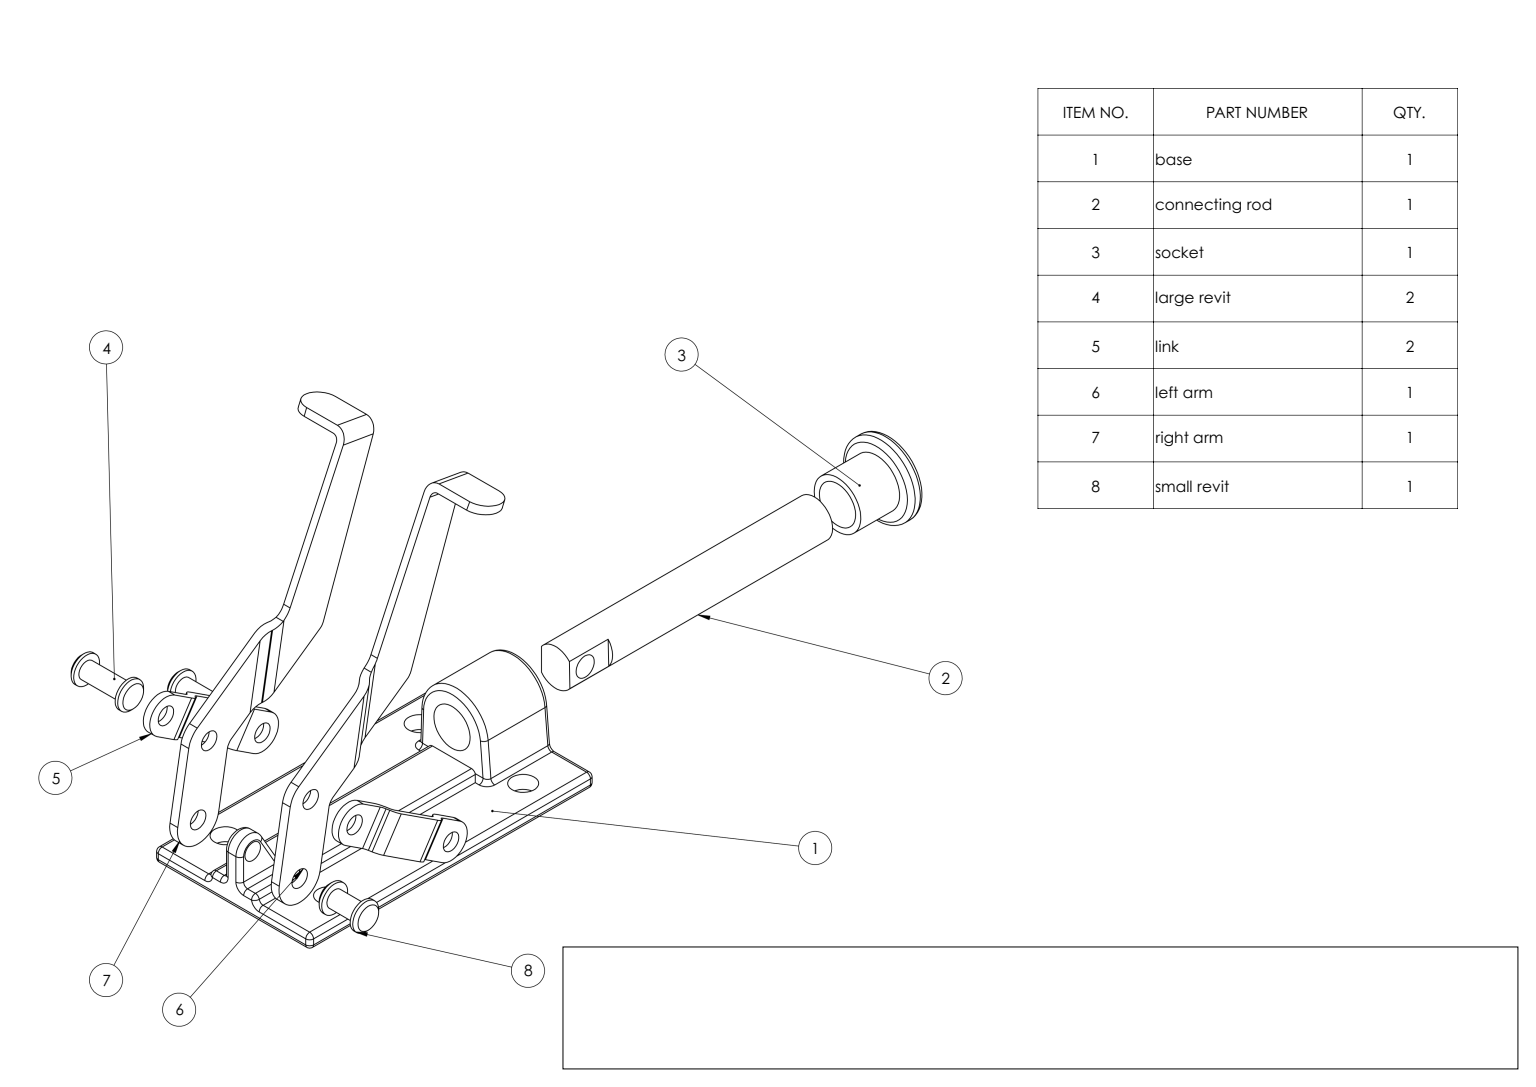
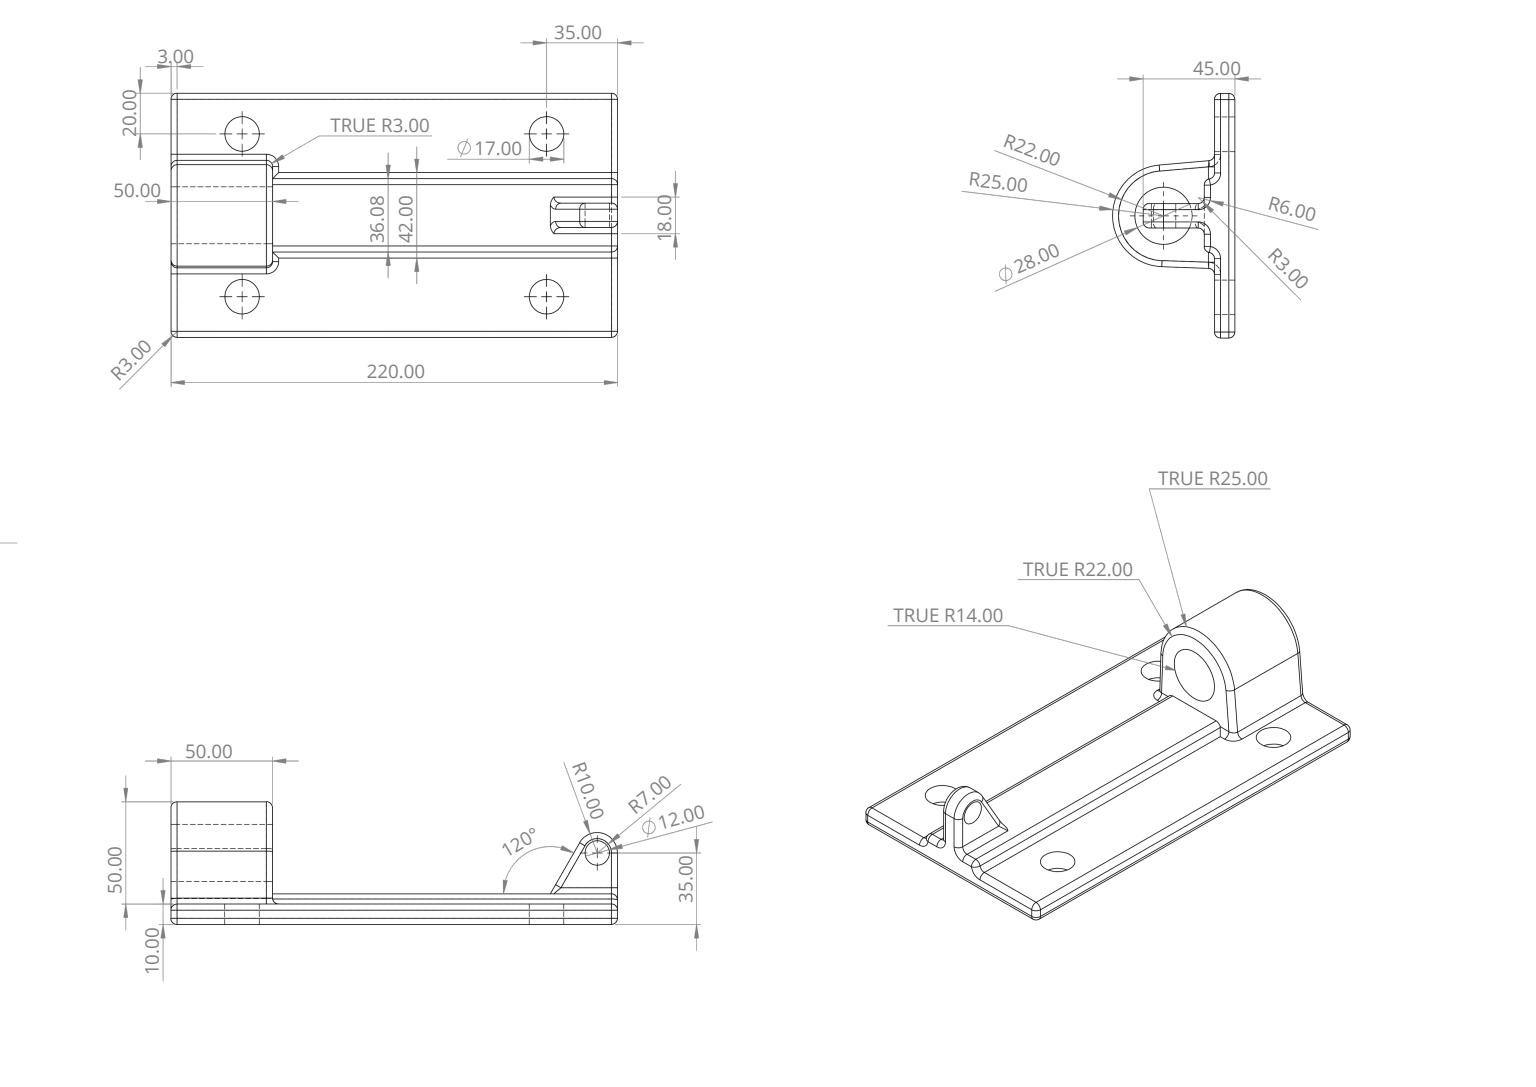
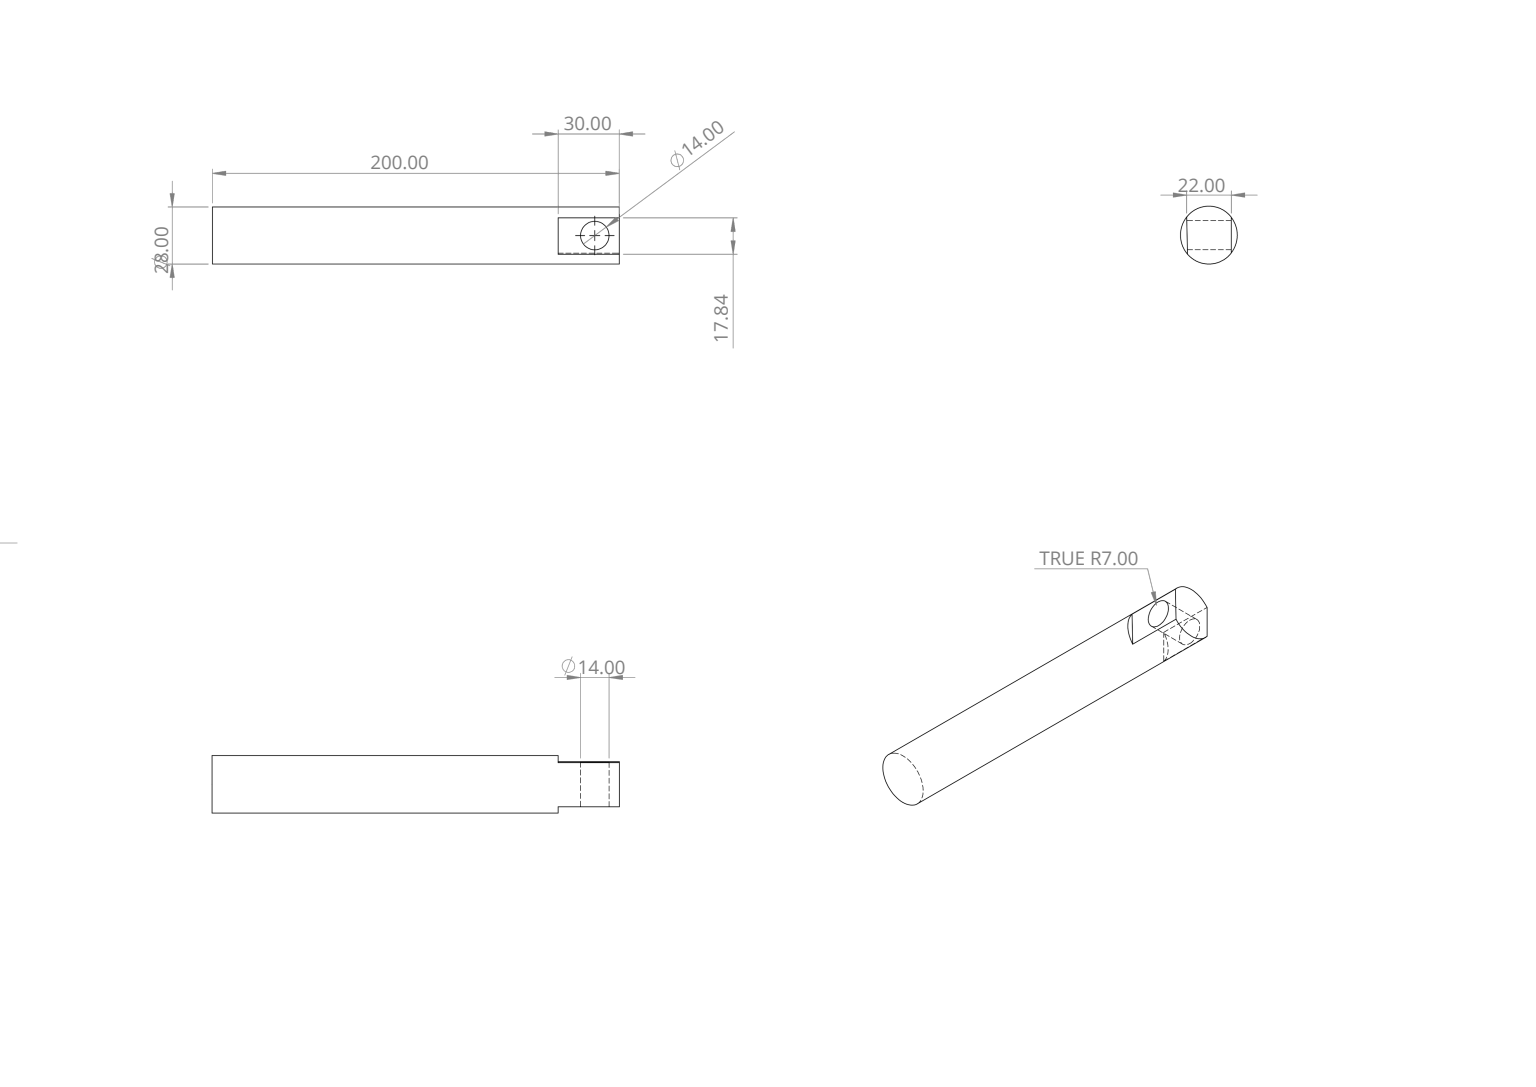
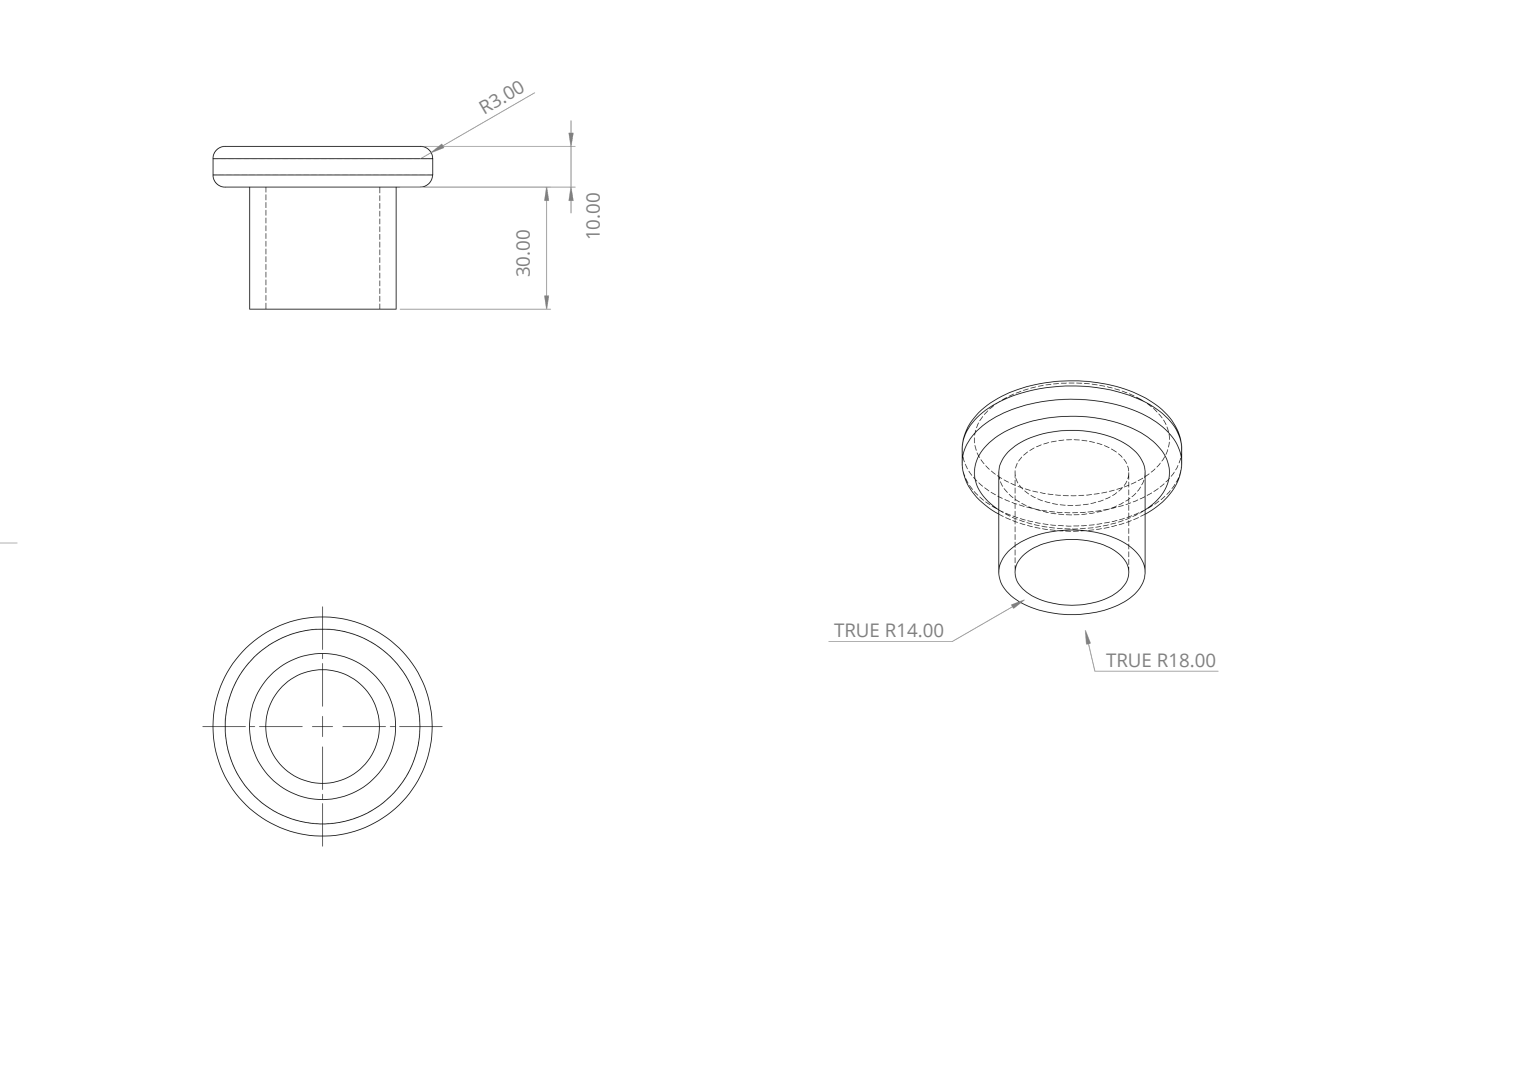
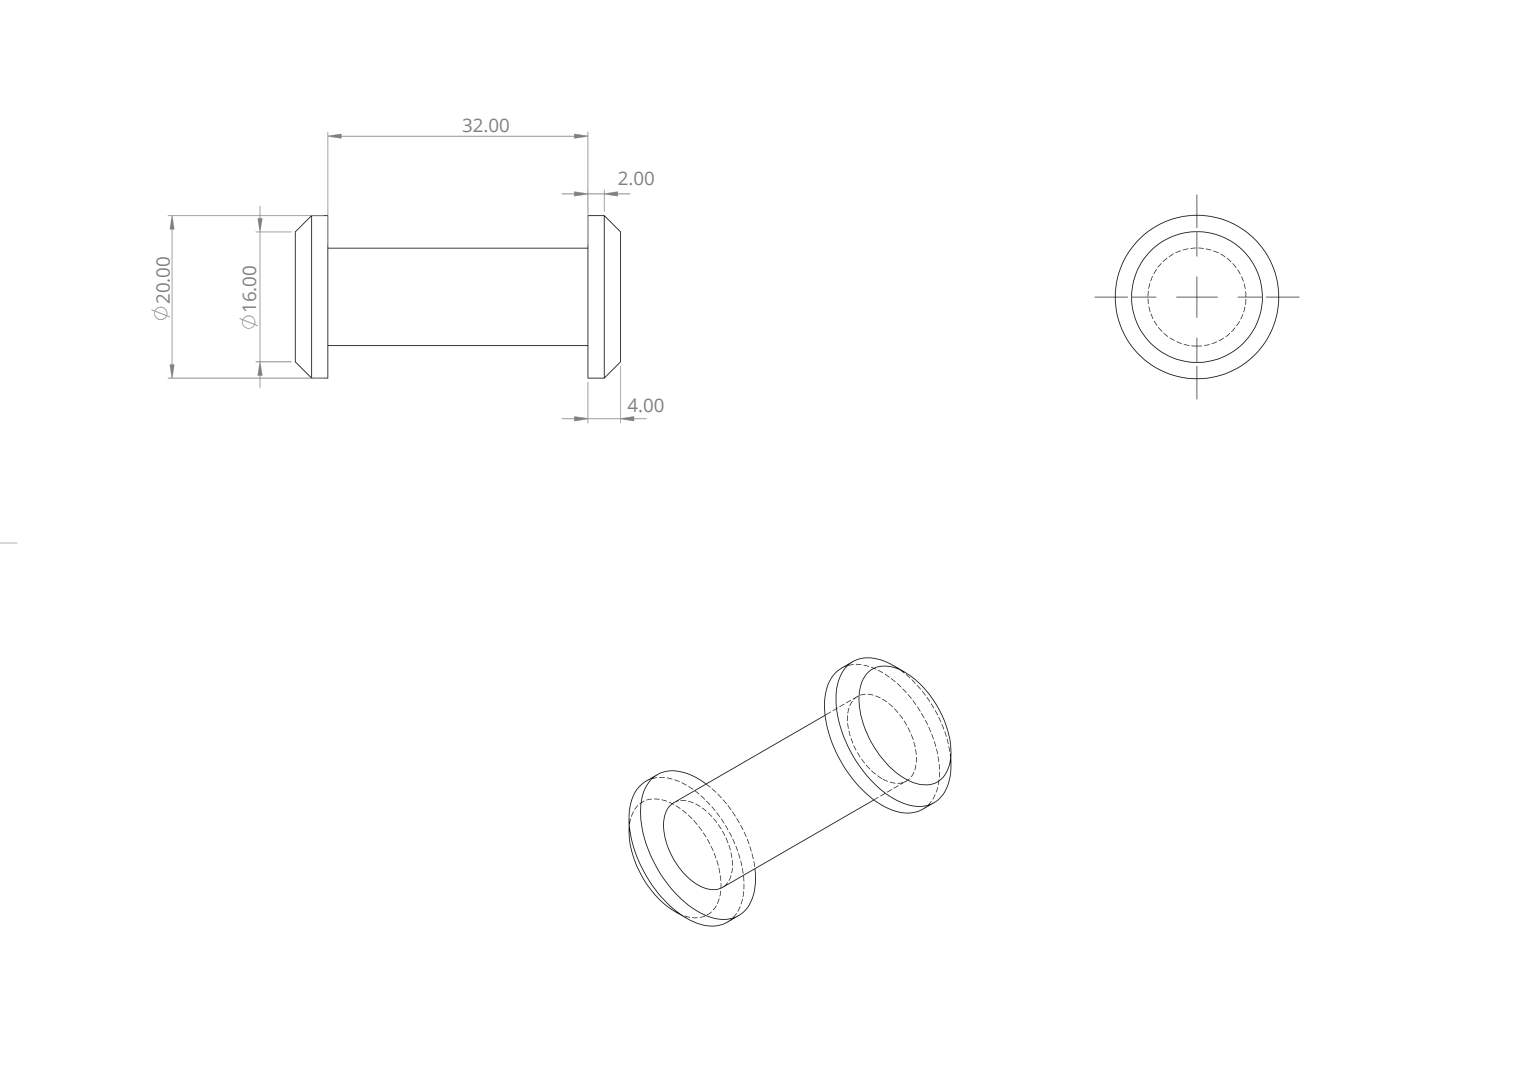
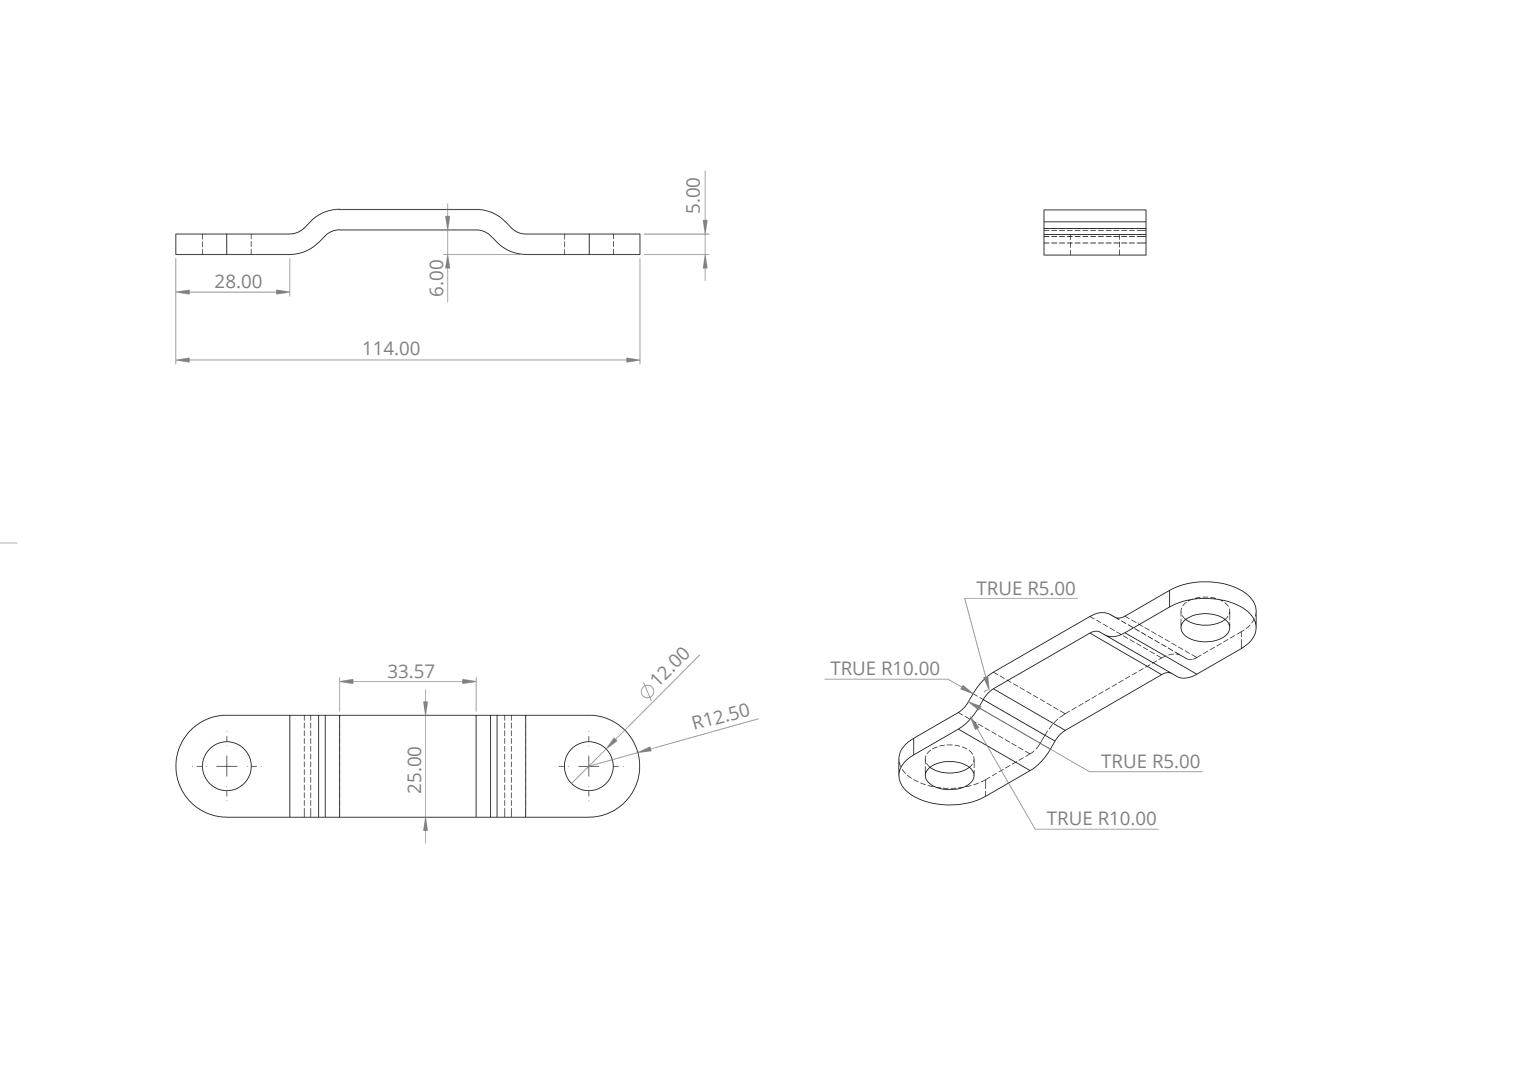
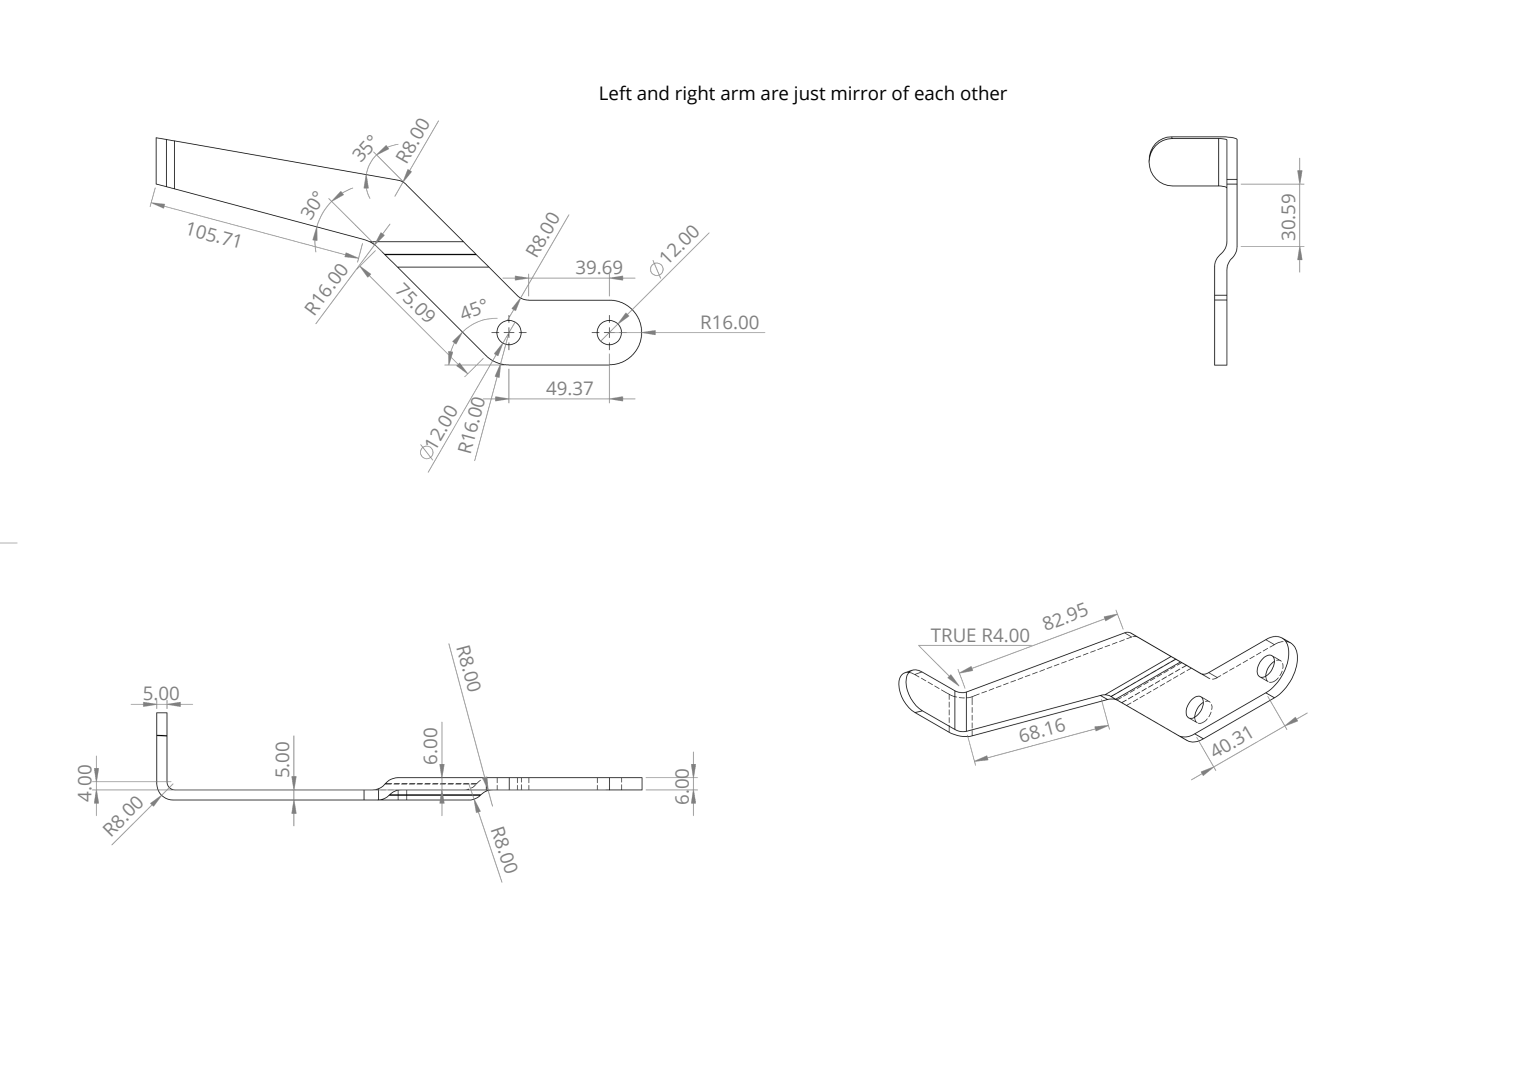
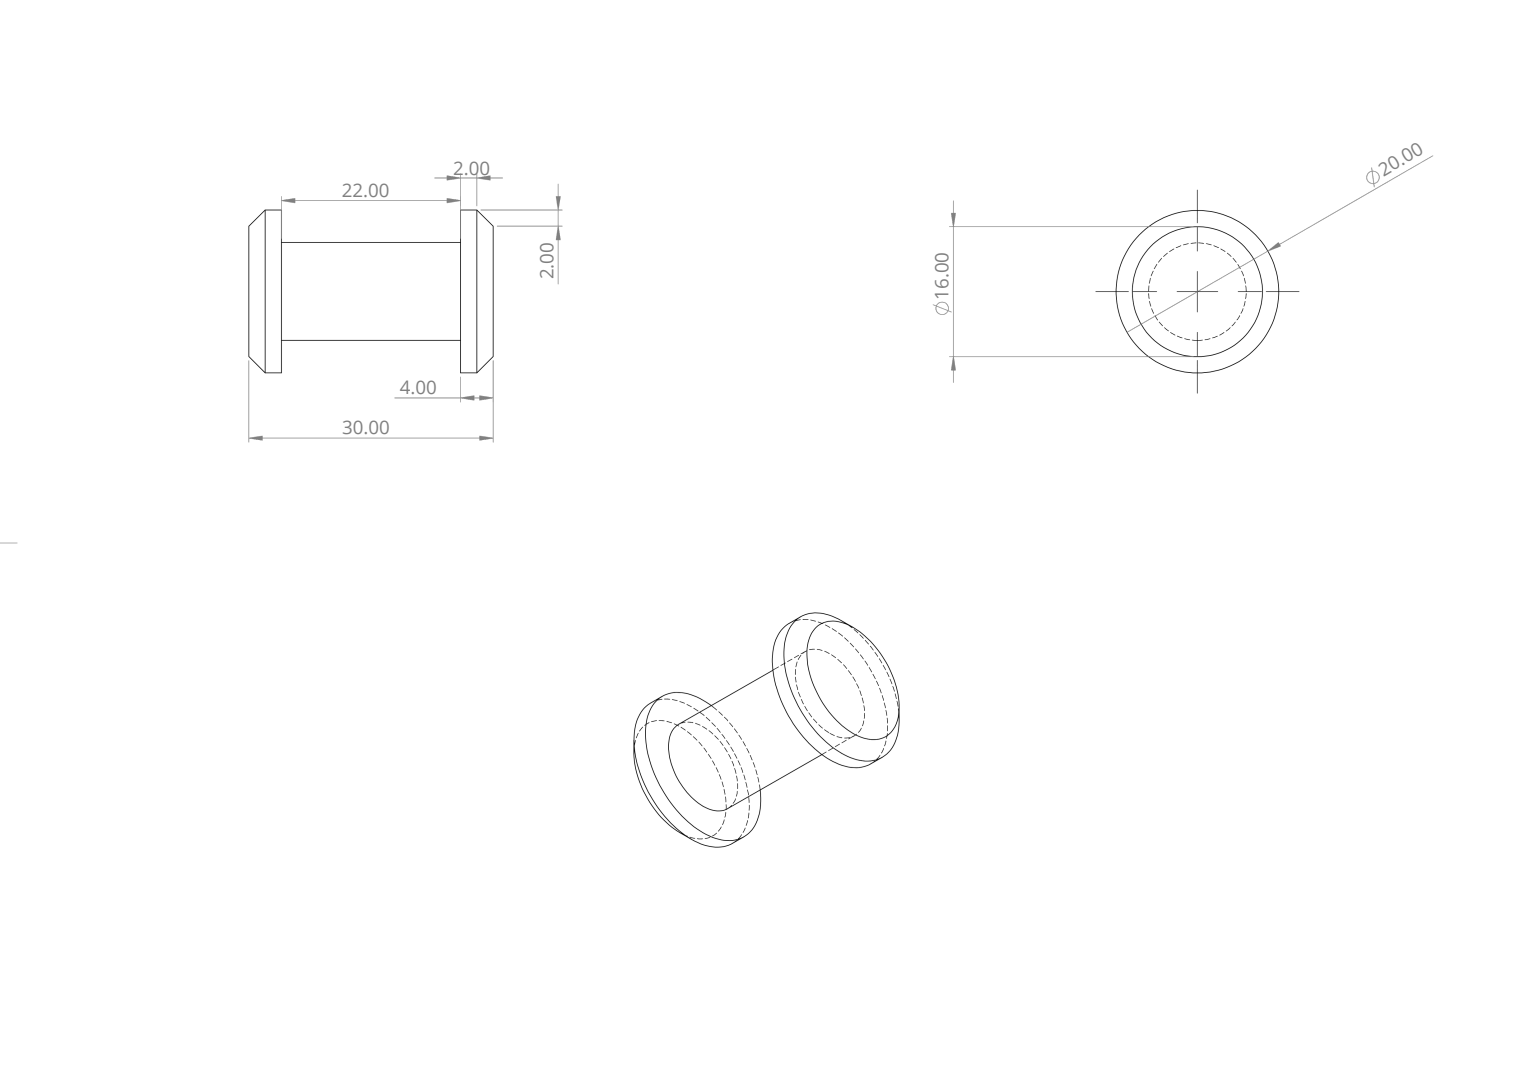
ISO-10303-21;
HEADER;
FILE_DESCRIPTION (('STEP AP214'),
    '1' );
FILE_NAME ('MAT-051',
    '2026-10-28T16:30:29',
    ( '' ),
    ( '' ),
    'SwSTEP 2.0',
    'SolidWorks 2025',
    '' );
FILE_SCHEMA (( 'AUTOMOTIVE_DESIGN' ));
ENDSEC;

DATA;
#1 = ORIENTED_EDGE ( 'NONE', *, *, #6027, .T. ) ;
#2 = AXIS2_PLACEMENT_3D ( 'NONE', #7401, #6721, #5569 ) ;
#3 = VERTEX_POINT ( 'NONE', #4491 ) ;
#4 = VECTOR ( 'NONE', #6644, 1000.000000000000000 ) ;
#5 = ADVANCED_FACE ( 'NONE', ( #5063 ), #903, .F. ) ;
#6 = CARTESIAN_POINT ( 'NONE',  ( -16.49999999999998934, 16.00000000000003908, 44.76505905230379767 ) ) ;
#7 = CARTESIAN_POINT ( 'NONE',  ( 27.24881022415626575, -213.6786602093778242, 88.60457046541063164 ) ) ;
#8 = ORIENTED_EDGE ( 'NONE', *, *, #2095, .F. ) ;
#9 = EDGE_CURVE ( 'NONE', #2534, #191, #5287, .T. ) ;
#10 = PRODUCT_CONTEXT ( 'NONE', #4822, 'mechanical' ) ;
#11 = AXIS2_PLACEMENT_3D ( 'NONE', #6403, #3479, #547 ) ;
#12 = DIRECTION ( 'NONE',  ( 1.000000000000000000, 0.000000000000000000, 0.000000000000000000 ) ) ;
#13 = EDGE_LOOP ( 'NONE', ( #3955, #3926, #2198, #6587 ) ) ;
#14 = AXIS2_PLACEMENT_3D ( 'NONE', #4631, #3929, #1078 ) ;
#15 = DIRECTION ( 'NONE',  ( 0.000000000000000000, 1.301042606982607490E-15, -1.000000000000000000 ) ) ;
#16 = DIRECTION ( 'NONE',  ( 1.000000000000000000, 0.000000000000000000, 0.000000000000000000 ) ) ;
#17 = CARTESIAN_POINT ( 'NONE',  ( 20.98347821072601960, -218.0630240738405519, 87.23510494545232064 ) ) ;
#18 = CARTESIAN_POINT ( 'NONE',  ( 20.97288657943079571, -223.0630240738404382, 88.26575131447681599 ) ) ;
#19 = CARTESIAN_POINT ( 'NONE',  ( -17.32280336819468047, -61.82280336819459166, 34.82280336819469824 ) ) ;
#20 = EDGE_CURVE ( 'NONE', #1964, #6977, #5721, .T. ) ;
#21 = PRODUCT_DEFINITION_CONTEXT ( 'detailed design', #2454, 'design' ) ;
#22 = EDGE_LOOP ( 'NONE', ( #2076, #4866, #387, #2753, #42, #1784, #2773 ) ) ;
#23 = AXIS2_PLACEMENT_3D ( 'NONE', #5950, #680, #1328 ) ;
#24 = ORIENTED_EDGE ( 'NONE', *, *, #3857, .T. ) ;
#25 = SURFACE_STYLE_FILL_AREA ( #599 ) ;
#26 = CARTESIAN_POINT ( 'NONE',  ( 3.000000000000002665, 0.000000000000000000, 35.00000000000000000 ) ) ;
#27 = LINE ( 'NONE', #5419, #4744 ) ;
#28 = CARTESIAN_POINT ( 'NONE',  ( 188.6380400399839061, 9.000000000000001776, 15.00000000000000888 ) ) ;
#29 = CARTESIAN_POINT ( 'NONE',  ( 30.00000000000000000, 0.000000000000000000, 0.000000000000000000 ) ) ;
#30 = AXIS2_PLACEMENT_3D ( 'NONE', #3464, #4542, #1564 ) ;
#31 = ORIENTED_EDGE ( 'NONE', *, *, #3655, .T. ) ;
#32 = ORIENTED_EDGE ( 'NONE', *, *, #3252, .F. ) ;
#33 = FACE_OUTER_BOUND ( 'NONE', #3649, .T. ) ;
#34 = DIRECTION ( 'NONE',  ( 1.000000000000000000, 2.465190328815661892E-32, -9.244463733058732095E-33 ) ) ;
#35 = ORIENTED_EDGE ( 'NONE', *, *, #1878, .T. ) ;
#36 = LINE ( 'NONE', #2385, #2482 ) ;
#37 = EDGE_CURVE ( 'NONE', #4344, #2575, #5917, .T. ) ;
#38 = SURFACE_STYLE_FILL_AREA ( #2961 ) ;
#39 = CARTESIAN_POINT ( 'NONE',  ( 200.0000000000000000, 11.00000000000000711, 8.660254037844383745 ) ) ;
#40 = EDGE_CURVE ( 'NONE', #3862, #1645, #5779, .T. ) ;
#41 = EDGE_LOOP ( 'NONE', ( #5508, #4352, #6797, #4752 ) ) ;
#42 = ORIENTED_EDGE ( 'NONE', *, *, #4968, .F. ) ;
#43 = AXIS2_PLACEMENT_3D ( 'NONE', #7599, #4696, #644 ) ;
#44 = PRODUCT_DEFINITION_SHAPE ( 'NONE', 'NONE',  #7602 ) ;
#45 = AXIS2_PLACEMENT_3D ( 'NONE', #5549, #210, #1347 ) ;
#46 = CARTESIAN_POINT ( 'NONE',  ( 209.9999999999999716, -3.000000000000000888, 35.00000000000000000 ) ) ;
#47 = CARTESIAN_POINT ( 'NONE',  ( 4.000000000000003553, 0.000000000000000000, 1.387778780781445676E-14 ) ) ;
#48 = ORIENTED_EDGE ( 'NONE', *, *, #3226, .T. ) ;
#49 = SHAPE_DEFINITION_REPRESENTATION ( #3722, #915 ) ;
#50 = DIRECTION ( 'NONE',  ( -1.000000000000000000, -0.000000000000000000, -0.000000000000000000 ) ) ;
#51 = DIRECTION ( 'NONE',  ( -1.084202172485505174E-16, 0.000000000000000000, 1.000000000000000000 ) ) ;
#52 = AXIS2_PLACEMENT_3D ( 'NONE', #1456, #3815, #1490 ) ;
#53 = AXIS2_PLACEMENT_3D ( 'NONE', #1297, #6992, #2338 ) ;
#54 = EDGE_CURVE ( 'NONE', #3265, #5898, #5654, .T. ) ;
#55 = ADVANCED_FACE ( 'NONE', ( #5029 ), #3220, .F. ) ;
#56 = ORIENTED_EDGE ( 'NONE', *, *, #1998, .T. ) ;
#57 = DIRECTION ( 'NONE',  ( 1.000000000000000000, 0.000000000000000000, 5.605193857299269528E-45 ) ) ;
#58 = CONICAL_SURFACE ( 'NONE', #5587, 8.000000000000003553, 0.7853981633974447263 ) ;
#59 = CARTESIAN_POINT ( 'NONE',  ( 30.00000000000000000, 0.000000000000000000, 0.000000000000000000 ) ) ;
#60 = CIRCLE ( 'NONE', #2634, 6.000000000000000888 ) ;
#61 = EDGE_LOOP ( 'NONE', ( #832, #7441, #3199, #4016 ) ) ;
#62 = DIRECTION ( 'NONE',  ( 0.000000000000000000, 0.000000000000000000, 1.000000000000000000 ) ) ;
#63 = CARTESIAN_POINT ( 'NONE',  ( 21.48754873573582813, -218.0630240738405803, 84.27726093503913773 ) ) ;
#64 = CARTESIAN_POINT ( 'NONE',  ( 3.000000000000002665, 30.03170604878415162, 13.00000000000001066 ) ) ;
#65 = FACE_OUTER_BOUND ( 'NONE', #2315, .T. ) ;
#66 = VECTOR ( 'NONE', #761, 1000.000000000000000 ) ;
#67 = TOROIDAL_SURFACE ( 'NONE', #1523, 24.00000000000000000, 3.000000000000000000 ) ;
#68 = VECTOR ( 'NONE', #7179, 1000.000000000000000 ) ;
#69 = ORIENTED_EDGE ( 'NONE', *, *, #4461, .T. ) ;
#70 = DIRECTION ( 'NONE',  ( -1.368455531567204171E-48, -0.1736481776669304422, -0.9848077530122080203 ) ) ;
#71 = CARTESIAN_POINT ( 'NONE',  ( 4.000000000000003553, 0.000000000000000000, 1.387778780781445676E-14 ) ) ;
#72 = DIRECTION ( 'NONE',  ( 0.000000000000000000, -0.03489949670250429292, -0.9993908270190956511 ) ) ;
#73 = PLANE ( 'NONE',  #5716 ) ;
#74 = DIRECTION ( 'NONE',  ( 0.000000000000000000, 0.000000000000000000, -1.000000000000000000 ) ) ;
#75 = AXIS2_PLACEMENT_3D ( 'NONE', #6050, #2005, #4940 ) ;
#76 = PRODUCT_DEFINITION_FORMATION_WITH_SPECIFIED_SOURCE ( 'ANY', '', #2239, .NOT_KNOWN. ) ;
#77 = CARTESIAN_POINT ( 'NONE',  ( 187.7594781219628999, -3.757281668791117468, 16.47828612039246465 ) ) ;
#78 = EDGE_LOOP ( 'NONE', ( #6432, #8, #7430, #5841, #2401, #1388, #6356, #5368 ) ) ;
#79 = VERTEX_POINT ( 'NONE', #3915 ) ;
#80 = EDGE_CURVE ( 'NONE', #4729, #1895, #4308, .T. ) ;
#81 = DIRECTION ( 'NONE',  ( -1.000000000000000000, 0.000000000000000000, -7.663350976776343357E-46 ) ) ;
#82 = CARTESIAN_POINT ( 'NONE',  ( 220.0000000000000000, -56.99999999999999289, 7.000000000000000888 ) ) ;
#83 = ORIENTED_EDGE ( 'NONE', *, *, #275, .T. ) ;
#84 = CARTESIAN_POINT ( 'NONE',  ( -53.48785751550376233, -228.1620966263577657, 74.64757051591519144 ) ) ;
#85 = AXIS2_PLACEMENT_3D ( 'NONE', #4576, #2304, #5803 ) ;
#86 = CARTESIAN_POINT ( 'NONE',  ( -30.49999999999998579, -218.0630240738404950, 95.20959099461346398 ) ) ;
#87 = DIRECTION ( 'NONE',  ( 1.000000000000000000, 0.000000000000000000, 0.000000000000000000 ) ) ;
#88 = ORIENTED_EDGE ( 'NONE', *, *, #483, .F. ) ;
#89 = ORIENTED_EDGE ( 'NONE', *, *, #875, .F. ) ;
#90 = AXIS2_PLACEMENT_3D ( 'NONE', #1507, #1400, #825 ) ;
#91 = EDGE_CURVE ( 'NONE', #2680, #1796, #4925, .T. ) ;
#92 = FACE_BOUND ( 'NONE', #5400, .T. ) ;
#93 = CARTESIAN_POINT ( 'NONE',  ( 17.75187451922245430, -223.0194114314941203, 73.26959217102432831 ) ) ;
#94 = ORIENTED_EDGE ( 'NONE', *, *, #5676, .T. ) ;
#95 = SHAPE_DEFINITION_REPRESENTATION ( #6712, #867 ) ;
#96 = DIRECTION ( 'NONE',  ( 3.379803290564627601E-16, -1.193489751472043281E-15, 1.000000000000000000 ) ) ;
#97 = SHAPE_REPRESENTATION ( 'socket', ( #1914 ), #434 ) ;
#98 = CARTESIAN_POINT ( 'NONE',  ( 217.0000000000000000, 20.99999999999999645, 13.00000000000000888 ) ) ;
#99 = AXIS2_PLACEMENT_3D ( 'NONE', #6628, #2937, #5286 ) ;
#100 = EDGE_LOOP ( 'NONE', ( #3777, #3352, #1778, #3381, #5909, #4070 ) ) ;
#101 = AXIS2_PLACEMENT_3D ( 'NONE', #3506, #6921, #4007 ) ;
#102 = CARTESIAN_POINT ( 'NONE',  ( -27.00000000000000000, 3.306546357697852550E-15, -3.000000000000002665 ) ) ;
#103 = EDGE_CURVE ( 'NONE', #1980, #3365, #5258, .T. ) ;
#104 = DIRECTION ( 'NONE',  ( -2.465190328815661892E-32, -1.000000000000000000, -1.193489751472043281E-15 ) ) ;
#105 = VERTEX_POINT ( 'NONE', #3335 ) ;
#106 = APPLICATION_CONTEXT ( 'automotive_design' ) ;
#107 = CYLINDRICAL_SURFACE ( 'NONE', #7534, 3.000000000000000000 ) ;
#108 = CARTESIAN_POINT ( 'NONE',  ( 0.000000000000000000, 0.000000000000000000, 0.000000000000000000 ) ) ;
#109 = CARTESIAN_POINT ( 'NONE',  ( 190.0729179104125137, 6.000000000000001776, 16.24264068711929454 ) ) ;
#110 = PLANE ( 'NONE',  #3658 ) ;
#111 = ADVANCED_FACE ( 'NONE', ( #6250 ), #4449, .F. ) ;
#112 = PLANE ( 'NONE',  #4971 ) ;
#113 = DIRECTION ( 'NONE',  ( 5.551115123125785167E-17, -0.7071067811865451302, 0.7071067811865499042 ) ) ;
#114 = CARTESIAN_POINT ( 'NONE',  ( -23.99999999999999289, 2.939152317953645922E-15, -3.000000000000002665 ) ) ;
#115 = CARTESIAN_POINT ( 'NONE',  ( 0.000000000000000000, 0.000000000000000000, 0.000000000000000000 ) ) ;
#116 = DIRECTION ( 'NONE',  ( -5.551115123125785167E-17, 0.7071067811865469066, 0.7071067811865482389 ) ) ;
#117 = ORIENTED_EDGE ( 'NONE', *, *, #841, .F. ) ;
#118 = ORIENTED_EDGE ( 'NONE', *, *, #6512, .T. ) ;
#119 = CARTESIAN_POINT ( 'NONE',  ( 217.0000000000000000, 56.99999999999999289, 2.149255132503604690E-14 ) ) ;
#120 = CARTESIAN_POINT ( 'NONE',  ( 36.00000000000000000, 0.000000000000000000, 1.387778780781445676E-14 ) ) ;
#121 = CARTESIAN_POINT ( 'NONE',  ( -70.24881022415625864, -213.6786602093778527, 88.60457046541068848 ) ) ;
#122 = PLANE ( 'NONE',  #5791 ) ;
#123 = CARTESIAN_POINT ( 'NONE',  ( -57.55570709107922767, -218.0630177787537605, 94.33845620223004858 ) ) ;
#124 = EDGE_CURVE ( 'NONE', #3147, #3862, #1554, .T. ) ;
#125 = ORIENTED_EDGE ( 'NONE', *, *, #2917, .T. ) ;
#126 =( BOUNDED_SURFACE ( )  B_SPLINE_SURFACE ( 3, 2, ( 
 ( #6358, #1115, #535 ),
 ( #7576, #4667, #7000 ),
 ( #5776, #2923, #7425 ),
 ( #2158, #4511, #999 ),
 ( #424, #6970, #2887 ),
 ( #5124, #7466, #686 ),
 ( #2497, #3699, #5310 ),
 ( #4202, #3048, #6003 ),
 ( #6470, #4707, #3588 ),
 ( #1190, #4166, #614 ) ),
 .UNSPECIFIED., .F., .F., .F. ) 
 B_SPLINE_SURFACE_WITH_KNOTS ( ( 4, 2, 2, 2, 4 ),
 ( 3, 3 ),
 ( 1.570796326794896558, 1.963495408493620697, 2.356194490192344837, 2.748893571891068976, 3.141592653589793116 ),
 ( 0.000000000000000000, 1.000000000000000000 ),
 .UNSPECIFIED. ) 
 GEOMETRIC_REPRESENTATION_ITEM ( )  RATIONAL_B_SPLINE_SURFACE ( (
 ( 1.000000000000000000, 0.7071067811865473507, 1.000000000000000000),
 ( 1.000000000000000000, 0.7087223175983969892, 1.000000000000000000),
 ( 1.000000000000000000, 0.7103306498028938432, 1.000000000000000000),
 ( 1.000000000000000000, 0.7132953257861496255, 1.000000000000000000),
 ( 1.000000000000000000, 0.7146502351234478301, 1.000000000000000000),
 ( 1.000000000000000000, 0.7169067290091972744, 1.000000000000000000),
 ( 1.000000000000000000, 0.7178075805514493313, 1.000000000000000000),
 ( 1.000000000000000000, 0.7190243029327590962, 1.000000000000000000),
 ( 1.000000000000000000, 0.7193412045353504425, 1.000000000000000000),
 ( 1.000000000000000000, 0.7193398003386524131, 1.000000000000000000) ) ) 
 REPRESENTATION_ITEM ( '' )  SURFACE ( )  );
#127 = EDGE_LOOP ( 'NONE', ( #2501, #1142, #956, #2609 ) ) ;
#128 = AXIS2_PLACEMENT_3D ( 'NONE', #2301, #7483, #6908 ) ;
#129 = CARTESIAN_POINT ( 'NONE',  ( 43.50000000000001421, 39.99999999999999289, 0.000000000000000000 ) ) ;
#130 = CARTESIAN_POINT ( 'NONE',  ( 27.04900473833201957, -225.0595978535630479, 79.55554317441176693 ) ) ;
#131 = VERTEX_POINT ( 'NONE', #5107 ) ;
#132 = CARTESIAN_POINT ( 'NONE',  ( 47.00000000000000000, 0.000000000000000000, 35.00000000000000000 ) ) ;
#133 = DIRECTION ( 'NONE',  ( 0.000000000000000000, -4.440892098500625373E-15, -1.000000000000000000 ) ) ;
#134 = CLOSED_SHELL ( 'NONE', ( #4385, #2935, #2103, #5773, #2173, #1411, #598, #7589, #2241, #2766, #3161, #4459, #4149, #7376, #3485, #1798, #883, #2489, #2656, #6564, #2581, #4183, #1712, #6059, #2477, #6043 ) ) ;
#135 = VECTOR ( 'NONE', #6601, 1000.000000000000000 ) ;
#136 = ORIENTED_EDGE ( 'NONE', *, *, #2636, .T. ) ;
#137 = DIRECTION ( 'NONE',  ( 0.000000000000000000, -1.000000000000000000, 0.000000000000000000 ) ) ;
#138 = AXIS2_PLACEMENT_3D ( 'NONE', #4135, #4211, #3123 ) ;
#139 = SPHERICAL_SURFACE ( 'NONE', #1773, 3.000000000000000000 ) ;
#140 = CARTESIAN_POINT ( 'NONE',  ( 26.49999999999999645, -39.99999999999999289, 0.000000000000000000 ) ) ;
#141 = FACE_OUTER_BOUND ( 'NONE', #3804, .T. ) ;
#142 = CARTESIAN_POINT ( 'NONE',  ( -16.49999999999996447, -57.68629150101509850, 30.68629150101520509 ) ) ;
#143 = EDGE_CURVE ( 'NONE', #589, #4118, #1720, .T. ) ;
#144 = ORIENTED_EDGE ( 'NONE', *, *, #928, .F. ) ;
#145 = CARTESIAN_POINT ( 'NONE',  ( -64.50000000000000000, -105.5631177942458407, 67.24940929526127320 ) ) ;
#146 = DIRECTION ( 'NONE',  ( 0.000000000000000000, 0.000000000000000000, 1.000000000000000000 ) ) ;
#147 = DIRECTION ( 'NONE',  ( -0.000000000000000000, 1.000000000000000000, 1.836970198721029934E-16 ) ) ;
#148 = LINE ( 'NONE', #4110, #1043 ) ;
#149 = CARTESIAN_POINT ( 'NONE',  ( -56.14779210138475918, -223.0637666356699071, 73.66476142575187680 ) ) ;
#150 = FACE_OUTER_BOUND ( 'NONE', #7477, .T. ) ;
#151 = VECTOR ( 'NONE', #2336, 1000.000000000000000 ) ;
#152 = EDGE_CURVE ( 'NONE', #3617, #6429, #5143, .T. ) ;
#153 = ORIENTED_EDGE ( 'NONE', *, *, #1028, .T. ) ;
#154 = EDGE_LOOP ( 'NONE', ( #6396, #3446, #5097, #6881, #3077, #1951, #4826, #5186 ) ) ;
#155 = DIRECTION ( 'NONE',  ( 1.853902270198407313E-44, 1.000000000000000000, 0.000000000000000000 ) ) ;
#156 = VECTOR ( 'NONE', #2539, 1000.000000000000000 ) ;
#157 = PLANE ( 'NONE',  #5099 ) ;
#158 = CARTESIAN_POINT ( 'NONE',  ( -70.08493024494319457, -223.4607234779400642, 79.16428349862681557 ) ) ;
#159 = CARTESIAN_POINT ( 'NONE',  ( -11.51602904742824762, -108.8525495989622556, 36.85254959896237636 ) ) ;
#160 = CARTESIAN_POINT ( 'NONE',  ( -57.59964905045998762, -218.0630227653799693, 94.31979920232429038 ) ) ;
#161 = ORIENTED_EDGE ( 'NONE', *, *, #5968, .F. ) ;
#162 = VERTEX_POINT ( 'NONE', #7062 ) ;
#163 = DIRECTION ( 'NONE',  ( 0.000000000000000000, 0.000000000000000000, 1.000000000000000000 ) ) ;
#164 = CARTESIAN_POINT ( 'NONE',  ( 10.17910001414514731, -221.3248423084432943, 72.81553374298380277 ) ) ;
#165 = ORIENTED_EDGE ( 'NONE', *, *, #3061, .F. ) ;
#166 = DIRECTION ( 'NONE',  ( -1.000000000000000000, 0.000000000000000000, 0.000000000000000000 ) ) ;
#167 = LINE ( 'NONE', #6090, #918 ) ;
#168 = EDGE_LOOP ( 'NONE', ( #6133, #5211, #83, #575 ) ) ;
#169 = VECTOR ( 'NONE', #1200, 1000.000000000000114 ) ;
#170 = FACE_BOUND ( 'NONE', #6243, .T. ) ;
#171 = EDGE_CURVE ( 'NONE', #5235, #6417, #2962, .T. ) ;
#172 = DIRECTION ( 'NONE',  ( 0.000000000000000000, 0.000000000000000000, 1.000000000000000000 ) ) ;
#173 = AXIS2_PLACEMENT_3D ( 'NONE', #4766, #2865, #1709 ) ;
#174 = DIRECTION ( 'NONE',  ( -0.000000000000000000, -0.000000000000000000, 1.000000000000000000 ) ) ;
#175 = LINE ( 'NONE', #5523, #4427 ) ;
#176 = AXIS2_PLACEMENT_3D ( 'NONE', #3789, #147, #6778 ) ;
#177=STYLED_ITEM('',(#7652),#6264);
#178 = CIRCLE ( 'NONE', #1154, 12.49999999999999645 ) ;
#179 =( BOUNDED_CURVE ( )  B_SPLINE_CURVE ( 3, ( #5830, #5717, #554, #2902 ),
 .UNSPECIFIED., .F., .T. ) 
 B_SPLINE_CURVE_WITH_KNOTS ( ( 4, 4 ),
 ( 1.637599047967249533, 2.356194490192343061 ),
 .UNSPECIFIED. ) 
 CURVE ( )  GEOMETRIC_REPRESENTATION_ITEM ( )  RATIONAL_B_SPLINE_CURVE ( ( 1.000000000000000000, 0.9574293250827446977, 0.9574293250827446977, 1.000000000000000000 ) ) 
 REPRESENTATION_ITEM ( '' )  );
#180 = DIRECTION ( 'NONE',  ( 0.000000000000000000, 1.000000000000000000, 0.000000000000000000 ) ) ;
#181 = EDGE_CURVE ( 'NONE', #5543, #2174, #5180, .T. ) ;
#182 = CYLINDRICAL_SURFACE ( 'NONE', #7539, 14.00000000000000533 ) ;
#183 = LINE ( 'NONE', #5993, #3215 ) ;
#184 = CARTESIAN_POINT ( 'NONE',  ( -26.50000000000003197, -39.68629150101523351, 15.99999999999998579 ) ) ;
#185 = CARTESIAN_POINT ( 'NONE',  ( -64.42620118284322928, -223.0639116415348155, 83.46765639585603935 ) ) ;
#186 = CARTESIAN_POINT ( 'NONE',  ( -21.50000000000000000, -215.0630240738404950, 94.68061005248806339 ) ) ;
#187 = AXIS2_PLACEMENT_3D ( 'NONE', #7080, #1809, #2958 ) ;
#188 = AXIS2_PLACEMENT_3D ( 'NONE', #5793, #16, #1672 ) ;
#189 = AXIS2_PLACEMENT_3D ( 'NONE', #7070, #4732, #2989 ) ;
#190 = ORIENTED_EDGE ( 'NONE', *, *, #5818, .T. ) ;
#191 = VERTEX_POINT ( 'NONE', #2258 ) ;
#192 = VECTOR ( 'NONE', #6509, 1000.000000000000114 ) ;
#193 =( GEOMETRIC_REPRESENTATION_CONTEXT ( 3 ) GLOBAL_UNCERTAINTY_ASSIGNED_CONTEXT ( ( #5332 ) ) GLOBAL_UNIT_ASSIGNED_CONTEXT ( ( #6857, #436, #2204 ) ) REPRESENTATION_CONTEXT ( 'NONE', 'WORKASPACE' ) );
#194 = CARTESIAN_POINT ( 'NONE',  ( 220.0000000000000000, -56.99999999999999289, 3.000000000000000444 ) ) ;
#195 = DIRECTION ( 'NONE',  ( 1.000000000000000000, 2.624548829666596736E-30, -9.231085635203017994E-31 ) ) ;
#196 = EDGE_CURVE ( 'NONE', #5318, #2388, #1106, .T. ) ;
#197 = EDGE_CURVE ( 'NONE', #2264, #3547, #4063, .T. ) ;
#198 = CARTESIAN_POINT ( 'NONE',  ( -53.17910001414514198, -221.3248423084432943, 72.81553374298380277 ) ) ;
#199 = CARTESIAN_POINT ( 'NONE',  ( -21.50000000000000000, -215.0630240738404950, 71.13768460387146320 ) ) ;
#200 = CARTESIAN_POINT ( 'NONE',  ( -60.96625293780100918, -218.0629435954679707, 92.08651146675032351 ) ) ;
#201 = AXIS2_PLACEMENT_3D ( 'NONE', #3407, #2248, #2699 ) ;
#202 = EDGE_LOOP ( 'NONE', ( #4107, #646, #7588, #6121 ) ) ;
#203 = ORIENTED_EDGE ( 'NONE', *, *, #3523, .T. ) ;
#204 = APPLICATION_CONTEXT ( 'automotive_design' ) ;
#205 = DIRECTION ( 'NONE',  ( 4.622231866529368100E-33, -2.600005424922769496E-32, 1.000000000000000000 ) ) ;
#206 = CARTESIAN_POINT ( 'NONE',  ( 27.00607124224622169, -226.9703646923684062, 80.02312588464758392 ) ) ;
#207 = EDGE_CURVE ( 'NONE', #5755, #6501, #4651, .T. ) ;
#208 = VERTEX_POINT ( 'NONE', #3488 ) ;
#209 = DIRECTION ( 'NONE',  ( 1.000000000000000000, 0.000000000000000000, 0.000000000000000000 ) ) ;
#210 = DIRECTION ( 'NONE',  ( -1.000000000000000000, 5.551115123125783935E-17, -4.237045877651919561E-33 ) ) ;
#211 = ORIENTED_EDGE ( 'NONE', *, *, #5767, .T. ) ;
#212 = CARTESIAN_POINT ( 'NONE',  ( -21.50000000000000000, -215.0630240738404950, 71.13768460387146320 ) ) ;
#213 = CARTESIAN_POINT ( 'NONE',  ( 0.000000000000000000, 0.000000000000000000, -3.000000000000002665 ) ) ;
#214 =( LENGTH_UNIT ( ) NAMED_UNIT ( * ) SI_UNIT ( .MILLI., .METRE. ) );
#215 = CARTESIAN_POINT ( 'NONE',  ( 6.500000000000007994, 12.50000000000001243, 4.999999999999995559 ) ) ;
#216 = CARTESIAN_POINT ( 'NONE',  ( 26.00000000000000000, 0.000000000000000000, 6.000000000000003553 ) ) ;
#217 = CYLINDRICAL_SURFACE ( 'NONE', #3317, 2.999999999999999112 ) ;
#218 = EDGE_LOOP ( 'NONE', ( #4919, #3639 ) ) ;
#219 = EDGE_CURVE ( 'NONE', #2614, #3744, #5836, .T. ) ;
#220 = VECTOR ( 'NONE', #5591, 1000.000000000000000 ) ;
#221 = CARTESIAN_POINT ( 'NONE',  ( 217.0000000000000000, 3.000000000000000888, 18.00000000000001066 ) ) ;
#222 = DIRECTION ( 'NONE',  ( 1.000000000000000000, 0.000000000000000000, 0.000000000000000000 ) ) ;
#223 = CARTESIAN_POINT ( 'NONE',  ( 25.00000000000002132, 0.000000000000000000, 4.999999999999992006 ) ) ;
#224 = CARTESIAN_POINT ( 'NONE',  ( -63.57431139349281324, -223.0630270109929825, 80.23469423765578767 ) ) ;
#225 = EDGE_LOOP ( 'NONE', ( #3231, #2812 ) ) ;
#226 = DIRECTION ( 'NONE',  ( 1.000000000000000000, 0.000000000000000000, 0.000000000000000000 ) ) ;
#227 = ORIENTED_EDGE ( 'NONE', *, *, #91, .T. ) ;
#228 = VERTEX_POINT ( 'NONE', #5257 ) ;
#229 = LINE ( 'NONE', #3078, #5734 ) ;
#230 = FACE_OUTER_BOUND ( 'NONE', #6873, .T. ) ;
#231 = DIRECTION ( 'NONE',  ( 0.000000000000000000, 0.9993908270190956511, -0.03489949670250429986 ) ) ;
#232 = CARTESIAN_POINT ( 'NONE',  ( -53.97164445155914336, -218.0630240738405234, 95.20959099461349240 ) ) ;
#233 = VERTEX_POINT ( 'NONE', #7594 ) ;
#234 = ADVANCED_FACE ( 'NONE', ( #2330 ), #7023, .F. ) ;
#235 = ORIENTED_EDGE ( 'NONE', *, *, #6293, .F. ) ;
#236 = LINE ( 'NONE', #5475, #4353 ) ;
#237 = CARTESIAN_POINT ( 'NONE',  ( 27.16044999292957840, -220.0996966972330995, 78.34180846956240885 ) ) ;
#238 = VERTEX_POINT ( 'NONE', #3137 ) ;
#239 = CARTESIAN_POINT ( 'NONE',  ( 220.0000000000000000, -56.99999999999999289, 10.00000000000000000 ) ) ;
#240 = CARTESIAN_POINT ( 'NONE',  ( 3.000000000000002665, -56.99999999999999289, 5.510910596163094486E-16 ) ) ;
#241 = EDGE_LOOP ( 'NONE', ( #6686, #1268 ) ) ;
#242 = EDGE_CURVE ( 'NONE', #131, #233, #7369, .T. ) ;
#243 = DIRECTION ( 'NONE',  ( 0.000000000000000000, -1.000000000000000000, -1.836970198721029934E-16 ) ) ;
#244 = DIRECTION ( 'NONE',  ( 1.000000000000000000, 0.000000000000000000, 0.000000000000000000 ) ) ;
#245 = VERTEX_POINT ( 'NONE', #3715 ) ;
#246 = DIRECTION ( 'NONE',  ( -0.000000000000000000, 1.000000000000000000, -0.000000000000000000 ) ) ;
#247 = LINE ( 'NONE', #3324, #6888 ) ;
#248 = AXIS2_PLACEMENT_3D ( 'NONE', #5219, #5144, #2259 ) ;
#249 = CARTESIAN_POINT ( 'NONE',  ( -64.50000000000000000, -99.90626354475342907, 72.90626354475362803 ) ) ;
#250 = ORIENTED_EDGE ( 'NONE', *, *, #171, .T. ) ;
#251 = VECTOR ( 'NONE', #6869, 1000.000000000000000 ) ;
#252 = CARTESIAN_POINT ( 'NONE',  ( 217.0000000000000000, 3.000000000000000000, 35.00000000000000000 ) ) ;
#253 = FACE_OUTER_BOUND ( 'NONE', #6708, .T. ) ;
#254 = CARTESIAN_POINT ( 'NONE',  ( 4.000000000000003553, 0.000000000000000000, 1.387778780781445676E-14 ) ) ;
#255 = CARTESIAN_POINT ( 'NONE',  ( -26.49999999999998934, -214.0630240738404666, 94.50428307177961074 ) ) ;
#256 = ADVANCED_FACE ( 'NONE', ( #6670 ), #4293, .F. ) ;
#257 = CARTESIAN_POINT ( 'NONE',  ( -55.78429200775497065, -223.0639285917831955, 73.57192785026977333 ) ) ;
#258 = VERTEX_POINT ( 'NONE', #1288 ) ;
#259 = CARTESIAN_POINT ( 'NONE',  ( 170.0000000000000000, 0.000000000000000000, 0.000000000000000000 ) ) ;
#260 = VECTOR ( 'NONE', #2250, 1000.000000000000000 ) ;
#261 = ORIENTED_EDGE ( 'NONE', *, *, #5274, .T. ) ;
#262 = ORIENTED_EDGE ( 'NONE', *, *, #1741, .F. ) ;
#263 = CARTESIAN_POINT ( 'NONE',  ( -10.49999999999996803, -60.68629150101523351, -11.31370849898472031 ) ) ;
#264 = ADVANCED_FACE ( 'NONE', ( #4799 ), #3938, .T. ) ;
#265 = CARTESIAN_POINT ( 'NONE',  ( 47.00000000000000000, 0.000000000000000000, 35.00000000000000000 ) ) ;
#266 = DIRECTION ( 'NONE',  ( -2.389881825834861318E-16, 0.7071067811865465735, -0.7071067811865484609 ) ) ;
#267 = CARTESIAN_POINT ( 'NONE',  ( 26.49999999999999645, 39.99999999999999289, 0.000000000000000000 ) ) ;
#268 = ORIENTED_EDGE ( 'NONE', *, *, #1167, .T. ) ;
#269 = ORIENTED_EDGE ( 'NONE', *, *, #1198, .F. ) ;
#270 = AXIS2_PLACEMENT_3D ( 'NONE', #1139, #3498, #377 ) ;
#271 = EDGE_CURVE ( 'NONE', #459, #258, #2406, .T. ) ;
#272 = FACE_BOUND ( 'NONE', #4560, .T. ) ;
#273 = CARTESIAN_POINT ( 'NONE',  ( 24.99999999999999289, 86.00000000000001421, 0.000000000000000000 ) ) ;
#274 = ORIENTED_EDGE ( 'NONE', *, *, #4877, .F. ) ;
#275 = EDGE_CURVE ( 'NONE', #2163, #5513, #3192, .T. ) ;
#276 = CARTESIAN_POINT ( 'NONE',  ( 0.000000000000000000, -5.510910596163110263E-16, 3.000000000000011102 ) ) ;
#277 = DIRECTION ( 'NONE',  ( 0.000000000000000000, 0.000000000000000000, -1.000000000000000000 ) ) ;
#278 = ORIENTED_EDGE ( 'NONE', *, *, #2137, .F. ) ;
#279 = DIRECTION ( 'NONE',  ( 0.000000000000000000, 0.000000000000000000, 1.000000000000000000 ) ) ;
#280 = CARTESIAN_POINT ( 'NONE',  ( 47.00000000000000000, 27.04312195450891565, 12.73853277175702203 ) ) ;
#281 = CARTESIAN_POINT ( 'NONE',  ( 25.00000000000000000, 31.53553390593274841, 6.464466094067257806 ) ) ;
#282 = ORIENTED_EDGE ( 'NONE', *, *, #4275, .F. ) ;
#283 = DIRECTION ( 'NONE',  ( 0.000000000000000000, -0.000000000000000000, 1.000000000000000000 ) ) ;
#284 = EDGE_CURVE ( 'NONE', #3833, #7386, #6600, .T. ) ;
#285 = DIRECTION ( 'NONE',  ( 0.4999999999999976130, 0.000000000000000000, 0.8660254037844399289 ) ) ;
#286 = ADVANCED_FACE ( 'NONE', ( #6562 ), #7173, .F. ) ;
#287 = CARTESIAN_POINT ( 'NONE',  ( 0.000000000000000000, 0.000000000000000000, 0.000000000000000000 ) ) ;
#288 = ORIENTED_EDGE ( 'NONE', *, *, #3333, .T. ) ;
#289 = CARTESIAN_POINT ( 'NONE',  ( 13.99999999999999645, 0.000000000000000000, -39.99999999999997868 ) ) ;
#290 = CIRCLE ( 'NONE', #2131, 2.999999999999999112 ) ;
#291 = LINE ( 'NONE', #789, #7056 ) ;
#292 = DIRECTION ( 'NONE',  ( -1.000000000000000000, -0.000000000000000000, -0.000000000000000000 ) ) ;
#293 = CARTESIAN_POINT ( 'NONE',  ( -62.09225886469350542, -223.0636046126283532, 77.65152759874978017 ) ) ;
#294 = CARTESIAN_POINT ( 'NONE',  ( 188.3757902719622450, -8.737358564324091859, 15.00000000000001066 ) ) ;
#295 = DIRECTION ( 'NONE',  ( -0.000000000000000000, 1.000000000000000000, -0.000000000000000000 ) ) ;
#296 = CIRCLE ( 'NONE', #4727, 23.99999999999999289 ) ;
#297 = ORIENTED_EDGE ( 'NONE', *, *, #778, .T. ) ;
#298 = ORIENTED_EDGE ( 'NONE', *, *, #6768, .T. ) ;
#299 = CARTESIAN_POINT ( 'NONE',  ( 26.49999999999999645, 39.99999999999999289, 0.000000000000000000 ) ) ;
#300 = AXIS2_PLACEMENT_3D ( 'NONE', #4781, #6581, #3079 ) ;
#301 = CARTESIAN_POINT ( 'NONE',  ( 217.0000000000000000, -20.99999999999999645, 7.000000000000008882 ) ) ;
#302 =( GEOMETRIC_REPRESENTATION_CONTEXT ( 3 ) GLOBAL_UNCERTAINTY_ASSIGNED_CONTEXT ( ( #2943 ) ) GLOBAL_UNIT_ASSIGNED_CONTEXT ( ( #2743, #3947, #5060 ) ) REPRESENTATION_CONTEXT ( 'NONE', 'WORKASPACE' ) );
#303 = AXIS2_PLACEMENT_3D ( 'NONE', #887, #7434, #5596 ) ;
#304 = DIRECTION ( 'NONE',  ( 3.379803290564628095E-16, 1.221245327087672392E-15, -1.000000000000000000 ) ) ;
#305 = ORIENTED_EDGE ( 'NONE', *, *, #103, .F. ) ;
#306 = CIRCLE ( 'NONE', #4740, 6.000000000000001776 ) ;
#307 = EDGE_CURVE ( 'NONE', #2650, #6611, #1827, .T. ) ;
#308 = VECTOR ( 'NONE', #3550, 1000.000000000000000 ) ;
#309 = CIRCLE ( 'NONE', #7190, 5.999999999999999112 ) ;
#310 = ORIENTED_EDGE ( 'NONE', *, *, #2775, .F. ) ;
#311 = DIRECTION ( 'NONE',  ( 0.000000000000000000, 0.000000000000000000, -1.000000000000000000 ) ) ;
#312 = VERTEX_POINT ( 'NONE', #2479 ) ;
#313 = CARTESIAN_POINT ( 'NONE',  ( 21.50000000000000000, 6.938893903907228378E-15, -16.00000000000001421 ) ) ;
#314 =( GEOMETRIC_REPRESENTATION_CONTEXT ( 3 ) GLOBAL_UNCERTAINTY_ASSIGNED_CONTEXT ( ( #560 ) ) GLOBAL_UNIT_ASSIGNED_CONTEXT ( ( #5090, #1047, #4439 ) ) REPRESENTATION_CONTEXT ( 'NONE', 'WORKASPACE' ) );
#315 = FACE_OUTER_BOUND ( 'NONE', #5801, .T. ) ;
#316 = VERTEX_POINT ( 'NONE', #2557 ) ;
#317 = ADVANCED_FACE ( 'NONE', ( #4185 ), #5986, .T. ) ;
#318 = DIRECTION ( 'NONE',  ( -1.000000000000000000, 1.294224922628222493E-31, -1.078147950931789264E-16 ) ) ;
#319 = CARTESIAN_POINT ( 'NONE',  ( 187.5739056480075533, 3.719611233821797036, 16.15686516701557807 ) ) ;
#320 = DIRECTION ( 'NONE',  ( 5.605193857299270773E-45, 0.000000000000000000, 1.000000000000000000 ) ) ;
#321 = ORIENTED_EDGE ( 'NONE', *, *, #3681, .F. ) ;
#322 = SHAPE_REPRESENTATION_RELATIONSHIP ( 'NONE' , 'NONE' ,  #7252, #961 ) ;
#323 = CARTESIAN_POINT ( 'NONE',  ( -60.67236366837563111, -212.7665347604139185, 94.27567702561840690 ) ) ;
#324 = CARTESIAN_POINT ( 'NONE',  ( -18.50000000000000355, 16.00000000000006750, 32.26953873476012546 ) ) ;
#325 =( NAMED_UNIT ( * ) SI_UNIT ( $, .STERADIAN. ) SOLID_ANGLE_UNIT ( ) );
#326 = ORIENTED_EDGE ( 'NONE', *, *, #2285, .T. ) ;
#327 = EDGE_CURVE ( 'NONE', #5270, #4738, #3066, .T. ) ;
#328 = DIRECTION ( 'NONE',  ( 1.000000000000000000, 0.000000000000000000, 0.000000000000000000 ) ) ;
#329 = FILL_AREA_STYLE_COLOUR ( '', #4859 ) ;
#330 = DIRECTION ( 'NONE',  ( -3.379803290564627601E-16, 0.000000000000000000, 1.000000000000000000 ) ) ;
#331 = CYLINDRICAL_SURFACE ( 'NONE', #4966, 6.000000000000000000 ) ;
#332 = CARTESIAN_POINT ( 'NONE',  ( -16.50000000000000711, -214.0630240738404382, 94.50428307177961074 ) ) ;
#333 = FACE_OUTER_BOUND ( 'NONE', #5193, .T. ) ;
#334 = AXIS2_PLACEMENT_3D ( 'NONE', #7079, #1650, #1144 ) ;
#335 = ORIENTED_EDGE ( 'NONE', *, *, #3931, .F. ) ;
#336 = EDGE_CURVE ( 'NONE', #5394, #4282, #7244, .T. ) ;
#337 = ORIENTED_EDGE ( 'NONE', *, *, #5469, .T. ) ;
#338 = DIRECTION ( 'NONE',  ( -1.000000000000000000, 0.000000000000000000, -7.663350976776343357E-46 ) ) ;
#339 = CARTESIAN_POINT ( 'NONE',  ( -16.50000000000000711, -223.0630240738404666, 96.09122589815579829 ) ) ;
#340 = CARTESIAN_POINT ( 'NONE',  ( -26.50000000000003197, 0.000000000000000000, -15.99999999999998579 ) ) ;
#341 = ORIENTED_EDGE ( 'NONE', *, *, #5136, .F. ) ;
#342 = ORIENTED_EDGE ( 'NONE', *, *, #7222, .F. ) ;
#343 = CARTESIAN_POINT ( 'NONE',  ( 50.00000000000000000, -17.91234734164656928, 13.00000000000000888 ) ) ;
#344 = ORIENTED_EDGE ( 'NONE', *, *, #6723, .F. ) ;
#345 = ADVANCED_FACE ( 'NONE', ( #141 ), #4259, .T. ) ;
#346 = PLANE ( 'NONE',  #6274 ) ;
#347 = CARTESIAN_POINT ( 'NONE',  ( -21.50000000000000000, -114.3401965514817960, 42.31370849898471675 ) ) ;
#348 = ORIENTED_EDGE ( 'NONE', *, *, #6825, .T. ) ;
#349 = CARTESIAN_POINT ( 'NONE',  ( -32.50000000000002842, 6.938893903907228378E-15, 0.000000000000000000 ) ) ;
#350 = DIRECTION ( 'NONE',  ( -1.000000000000000000, -2.624548829666596736E-30, 9.231085635203017994E-31 ) ) ;
#351 = ORIENTED_EDGE ( 'NONE', *, *, #1487, .T. ) ;
#352 = DIRECTION ( 'NONE',  ( 0.000000000000000000, 0.000000000000000000, 1.000000000000000000 ) ) ;
#353 = CARTESIAN_POINT ( 'NONE',  ( -60.80066350777957496, -221.4565245236573787, 95.80795668296072165 ) ) ;
#354 = CARTESIAN_POINT ( 'NONE',  ( 203.9378221735088914, 6.000000000000000000, 38.49999999999997868 ) ) ;
#355 = CARTESIAN_POINT ( 'NONE',  ( 217.0000000000000000, 56.99999999999999289, 3.000000000000021316 ) ) ;
#356 = ORIENTED_EDGE ( 'NONE', *, *, #3273, .T. ) ;
#357 = ORIENTED_EDGE ( 'NONE', *, *, #284, .T. ) ;
#358 = CARTESIAN_POINT ( 'NONE',  ( 47.00000000000000000, 21.91628335801839356, 36.91742634044857141 ) ) ;
#359 = SURFACE_STYLE_FILL_AREA ( #942 ) ;
#360 = FACE_OUTER_BOUND ( 'NONE', #1701, .T. ) ;
#361 = CIRCLE ( 'NONE', #1960, 6.000000000000000888 ) ;
#362 = CARTESIAN_POINT ( 'NONE',  ( -21.50000000000000000, -223.0630240738404666, 96.09122589815579829 ) ) ;
#363 = EDGE_CURVE ( 'NONE', #7339, #580, #4329, .T. ) ;
#364 = CARTESIAN_POINT ( 'NONE',  ( -58.06022122231924953, -223.0629902891046754, 95.07455849590682817 ) ) ;
#365 = CARTESIAN_POINT ( 'NONE',  ( 25.00000000000000000, 40.21320343559644783, 10.99999999999999467 ) ) ;
#366 = PLANE ( 'NONE',  #3453 ) ;
#367 = ADVANCED_FACE ( 'NONE', ( #3099 ), #3945, .T. ) ;
#368 = CARTESIAN_POINT ( 'NONE',  ( -60.60568960484322787, -218.0627689607302386, 92.42072044652158525 ) ) ;
#369 = AXIS2_PLACEMENT_3D ( 'NONE', #2064, #7334, #2026 ) ;
#370 = VECTOR ( 'NONE', #1803, 1000.000000000000000 ) ;
#371 = ORIENTED_EDGE ( 'NONE', *, *, #1452, .T. ) ;
#372 = ORIENTED_EDGE ( 'NONE', *, *, #3640, .F. ) ;
#373 = LINE ( 'NONE', #6957, #4602 ) ;
#374 = CARTESIAN_POINT ( 'NONE',  ( 170.0000000000000000, 11.00000000000000533, -8.660254037844387298 ) ) ;
#375 = CARTESIAN_POINT ( 'NONE',  ( 43.50000000000001421, -39.99999999999999289, 0.000000000000000000 ) ) ;
#376 = CONICAL_SURFACE ( 'NONE', #7132, 7.999999999999986677, 0.7853981633974473908 ) ;
#377 = DIRECTION ( 'NONE',  ( 0.000000000000000000, 0.000000000000000000, 1.000000000000000000 ) ) ;
#378 = ADVANCED_FACE ( 'NONE', ( #5943 ), #675, .F. ) ;
#379 = PRODUCT_RELATED_PRODUCT_CATEGORY ( 'part', '', ( #6529 ) ) ;
#380 = ORIENTED_EDGE ( 'NONE', *, *, #5109, .T. ) ;
#381 = VECTOR ( 'NONE', #2727, 1000.000000000000000 ) ;
#382 = ORIENTED_EDGE ( 'NONE', *, *, #143, .F. ) ;
#383 = CARTESIAN_POINT ( 'NONE',  ( 220.0000000000000000, 9.000000000000001776, 12.00000000000000711 ) ) ;
#384 = ORIENTED_EDGE ( 'NONE', *, *, #1937, .F. ) ;
#385 = CARTESIAN_POINT ( 'NONE',  ( 18.50000000000000711, 101.5000000000000000, -1.214306433183764966E-14 ) ) ;
#386 = CARTESIAN_POINT ( 'NONE',  ( -26.50000000000003197, -99.90626354475344328, 72.90626354475362803 ) ) ;
#387 = ORIENTED_EDGE ( 'NONE', *, *, #1165, .F. ) ;
#388 = DIRECTION ( 'NONE',  ( 0.000000000000000000, 0.000000000000000000, 1.000000000000000000 ) ) ;
#389 = FACE_BOUND ( 'NONE', #4788, .T. ) ;
#390 = EDGE_LOOP ( 'NONE', ( #4887, #963, #5814, #6487, #1201, #1973, #2378, #1958, #3679, #4178 ) ) ;
#391 = DIRECTION ( 'NONE',  ( 1.789239426140502911E-30, 1.000000000000000000, -6.417623122419729086E-31 ) ) ;
#392 = AXIS2_PLACEMENT_3D ( 'NONE', #5521, #246, #4948 ) ;
#393 = CARTESIAN_POINT ( 'NONE',  ( -53.50256896896190995, -223.7273137069649636, 96.20835808348057583 ) ) ;
#394 = LINE ( 'NONE', #3907, #3581 ) ;
#395 = DIRECTION ( 'NONE',  ( 1.000000000000000000, 0.000000000000000000, 0.000000000000000000 ) ) ;
#396 = ORIENTED_EDGE ( 'NONE', *, *, #40, .T. ) ;
#397 = ORIENTED_EDGE ( 'NONE', *, *, #2841, .F. ) ;
#398 = ADVANCED_FACE ( 'NONE', ( #5094 ), #5522, .F. ) ;
#399 = PLANE ( 'NONE',  #3904 ) ;
#400 = CARTESIAN_POINT ( 'NONE',  ( 190.3479161152068286, 6.383114783474912457, 16.48079611847125392 ) ) ;
#401 = CARTESIAN_POINT ( 'NONE',  ( -54.18008430849435086, -223.0630240738405519, 96.09122589815579829 ) ) ;
#402 = CARTESIAN_POINT ( 'NONE',  ( -32.50000000000002132, -39.68629150101521219, 24.00000000000002132 ) ) ;
#403 = FACE_BOUND ( 'NONE', #5032, .T. ) ;
#404 = CARTESIAN_POINT ( 'NONE',  ( 53.00000000000002132, 60.00000000000000000, 10.00000000000002309 ) ) ;
#405 = ORIENTED_EDGE ( 'NONE', *, *, #591, .F. ) ;
#406 = EDGE_CURVE ( 'NONE', #5445, #6726, #3208, .T. ) ;
#407 = EDGE_LOOP ( 'NONE', ( #5425, #6759, #1885, #3552 ) ) ;
#408 = DIRECTION ( 'NONE',  ( 1.000000000000000000, 0.000000000000000000, 0.000000000000000000 ) ) ;
#409 = CYLINDRICAL_SURFACE ( 'NONE', #3526, 2.999999999999999112 ) ;
#410 = CARTESIAN_POINT ( 'NONE',  ( 12.50000000000000355, 101.5000000000000000, 0.000000000000000000 ) ) ;
#411 = DIRECTION ( 'NONE',  ( 3.379803290564627601E-16, 0.000000000000000000, 1.000000000000000000 ) ) ;
#412 = FACE_OUTER_BOUND ( 'NONE', #6747, .T. ) ;
#413 = CIRCLE ( 'NONE', #1764, 6.000000000000001776 ) ;
#414 = AXIS2_PLACEMENT_3D ( 'NONE', #6878, #3960, #1027 ) ;
#415 = EDGE_LOOP ( 'NONE', ( #4669, #5784, #1959, #6893 ) ) ;
#416 = ORIENTED_EDGE ( 'NONE', *, *, #5323, .T. ) ;
#417 = CIRCLE ( 'NONE', #4735, 10.00000000000000355 ) ;
#418 = MECHANICAL_DESIGN_GEOMETRIC_PRESENTATION_REPRESENTATION (  '', ( #786 ), #5839 ) ;
#419 = EDGE_CURVE ( 'NONE', #5657, #1381, #4950, .T. ) ;
#420 = CIRCLE ( 'NONE', #303, 6.000000000000001776 ) ;
#421 =( BOUNDED_CURVE ( )  B_SPLINE_CURVE ( 3, ( #2509, #4253, #5516, #3784 ),
 .UNSPECIFIED., .F., .T. ) 
 B_SPLINE_CURVE_WITH_KNOTS ( ( 4, 4 ),
 ( 4.712388980384687898, 5.585053606381843672 ),
 .UNSPECIFIED. ) 
 CURVE ( )  GEOMETRIC_REPRESENTATION_ITEM ( )  RATIONAL_B_SPLINE_CURVE ( ( 1.000000000000000000, 0.9375385246911012160, 0.9375385246911012160, 1.000000000000000000 ) ) 
 REPRESENTATION_ITEM ( '' )  );
#422 = LINE ( 'NONE', #383, #2018 ) ;
#423 = ORIENTED_EDGE ( 'NONE', *, *, #430, .F. ) ;
#424 = CARTESIAN_POINT ( 'NONE',  ( 51.79800105182081182, -26.47119478651012514, 10.00000000000000533 ) ) ;
#425 = CARTESIAN_POINT ( 'NONE',  ( 51.46767767233086488, -19.46767767233084712, 10.00000000000001066 ) ) ;
#426 = CIRCLE ( 'NONE', #7052, 3.000000000000004885 ) ;
#427 = AXIS2_PLACEMENT_3D ( 'NONE', #4064, #2862, #1091 ) ;
#428 = AXIS2_PLACEMENT_3D ( 'NONE', #4264, #6030, #4882 ) ;
#429 = VERTEX_POINT ( 'NONE', #5560 ) ;
#430 = EDGE_CURVE ( 'NONE', #6206, #797, #247, .T. ) ;
#431 = AXIS2_PLACEMENT_3D ( 'NONE', #4321, #1460, #846 ) ;
#432 = CARTESIAN_POINT ( 'NONE',  ( -29.64230087749237441, 16.00000000000007105, 38.39789427971190605 ) ) ;
#433 = DIRECTION ( 'NONE',  ( -1.000000000000000000, 0.000000000000000000, 0.000000000000000000 ) ) ;
#434 =( GEOMETRIC_REPRESENTATION_CONTEXT ( 3 ) GLOBAL_UNCERTAINTY_ASSIGNED_CONTEXT ( ( #6415 ) ) GLOBAL_UNIT_ASSIGNED_CONTEXT ( ( #1708, #3828, #5557 ) ) REPRESENTATION_CONTEXT ( 'NONE', 'WORKASPACE' ) );
#435 = ORIENTED_EDGE ( 'NONE', *, *, #7404, .T. ) ;
#436 =( NAMED_UNIT ( * ) PLANE_ANGLE_UNIT ( ) SI_UNIT ( $, .RADIAN. ) );
#437 = DIRECTION ( 'NONE',  ( 0.000000000000000000, 0.03489949670250403618, 0.9993908270190956511 ) ) ;
#438 = LINE ( 'NONE', #1161, #260 ) ;
#439 = DIRECTION ( 'NONE',  ( -2.465190328815661892E-32, -1.000000000000000000, -1.193489751472043281E-15 ) ) ;
#440 = ORIENTED_EDGE ( 'NONE', *, *, #3673, .F. ) ;
#441 = VERTEX_POINT ( 'NONE', #6745 ) ;
#442 = PLANE ( 'NONE',  #948 ) ;
#443 = CARTESIAN_POINT ( 'NONE',  ( -16.49999999999996447, -39.68629150101519087, 15.99999999999998579 ) ) ;
#444 = AXIS2_PLACEMENT_3D ( 'NONE', #3267, #7341, #2187 ) ;
#445 = CARTESIAN_POINT ( 'NONE',  ( 188.6338938035227102, 8.633158558239344416, 14.99640925390055557 ) ) ;
#446 = CARTESIAN_POINT ( 'NONE',  ( -61.66056754332376499, -223.0629452613760577, 92.37656864897833486 ) ) ;
#447 = CARTESIAN_POINT ( 'NONE',  ( 35.00000000000000000, -39.99999999999999289, 0.000000000000000000 ) ) ;
#448 = FACE_OUTER_BOUND ( 'NONE', #7282, .T. ) ;
#449 = EDGE_CURVE ( 'NONE', #3729, #4344, #2629, .T. ) ;
#450 = CARTESIAN_POINT ( 'NONE',  ( -63.60296540135762200, -218.0630256771593167, 79.14794472078611420 ) ) ;
#451 = ORIENTED_EDGE ( 'NONE', *, *, #1471, .T. ) ;
#452 = VERTEX_POINT ( 'NONE', #7285 ) ;
#453 = FACE_OUTER_BOUND ( 'NONE', #2431, .T. ) ;
#454 = CARTESIAN_POINT ( 'NONE',  ( 30.00000000000000000, 0.000000000000000000, 0.000000000000000000 ) ) ;
#455 = CARTESIAN_POINT ( 'NONE',  ( 37.99999999999998579, 0.000000000000000000, 1.387778780781445676E-14 ) ) ;
#456 = CARTESIAN_POINT ( 'NONE',  ( 30.00000000000000000, 1.224646799147353651E-15, -10.00000000000000355 ) ) ;
#457 = VECTOR ( 'NONE', #1691, 1000.000000000000000 ) ;
#458 = ORIENTED_EDGE ( 'NONE', *, *, #2945, .F. ) ;
#459 = VERTEX_POINT ( 'NONE', #7439 ) ;
#460 = FACE_BOUND ( 'NONE', #2532, .T. ) ;
#461 = FACE_OUTER_BOUND ( 'NONE', #4848, .T. ) ;
#462 = ORIENTED_EDGE ( 'NONE', *, *, #2114, .F. ) ;
#463 = LINE ( 'NONE', #5158, #995 ) ;
#464 = FACE_OUTER_BOUND ( 'NONE', #1341, .T. ) ;
#465 = ADVANCED_FACE ( 'NONE', ( #3830 ), #376, .T. ) ;
#466 = ORIENTED_EDGE ( 'NONE', *, *, #5900, .F. ) ;
#467 = DIRECTION ( 'NONE',  ( 0.000000000000000000, 0.000000000000000000, -1.000000000000000000 ) ) ;
#468 = ORIENTED_EDGE ( 'NONE', *, *, #3972, .F. ) ;
#469 = CARTESIAN_POINT ( 'NONE',  ( -53.29386626619290723, -219.0153713307822443, 95.37751551101598579 ) ) ;
#470 = CARTESIAN_POINT ( 'NONE',  ( 217.0000000000000000, 60.00000000000000000, 3.000000000000021760 ) ) ;
#471 = DIRECTION ( 'NONE',  ( 0.8660254037844404840, 0.000000000000000000, -0.4999999999999968359 ) ) ;
#472 = VERTEX_POINT ( 'NONE', #4991 ) ;
#473 = ADVANCED_FACE ( 'NONE', ( #2054 ), #6822, .T. ) ;
#474 = ORIENTED_EDGE ( 'NONE', *, *, #3322, .T. ) ;
#475 = ADVANCED_FACE ( 'NONE', ( #6202 ), #7356, .F. ) ;
#476 = CARTESIAN_POINT ( 'NONE',  ( 47.00000000000000000, -28.78532416918554304, 10.00000000000000711 ) ) ;
#477 = CARTESIAN_POINT ( 'NONE',  ( 192.1021416551216419, 6.000000000000000888, 18.00000000000001066 ) ) ;
#478 = CARTESIAN_POINT ( 'NONE',  ( -61.82581114567872760, -223.0628484516971923, 92.18631465749969323 ) ) ;
#479 = CARTESIAN_POINT ( 'NONE',  ( 13.86971907638974244, -223.0630240738404382, 73.89376335044022426 ) ) ;
#480 = LINE ( 'NONE', #4569, #5650 ) ;
#481 = CARTESIAN_POINT ( 'NONE',  ( -57.51269236885188008, -218.0630271768473278, 72.88129350492478409 ) ) ;
#482 = ORIENTED_EDGE ( 'NONE', *, *, #4932, .F. ) ;
#483 = EDGE_CURVE ( 'NONE', #4729, #5898, #394, .T. ) ;
#484 = CARTESIAN_POINT ( 'NONE',  ( 217.0000000000000000, 56.99999999999999289, 3.000000000000021760 ) ) ;
#485 = DIRECTION ( 'NONE',  ( 0.000000000000000000, 0.000000000000000000, -1.000000000000000000 ) ) ;
#486 = CARTESIAN_POINT ( 'NONE',  ( 25.00000000000000711, 77.32233047033632545, 4.535533905932713772 ) ) ;
#487 = CARTESIAN_POINT ( 'NONE',  ( 50.04196010845020481, -18.04196010845019060, 12.50000000000000533 ) ) ;
#488 = CARTESIAN_POINT ( 'NONE',  ( 25.00000000000000711, 40.21320343559642652, 0.9999999999999956701 ) ) ;
#489 = CIRCLE ( 'NONE', #2947, 7.999999999999986677 ) ;
#490 = ORIENTED_EDGE ( 'NONE', *, *, #3084, .F. ) ;
#491 = ORIENTED_EDGE ( 'NONE', *, *, #3019, .T. ) ;
#492 = EDGE_CURVE ( 'NONE', #6160, #5563, #3866, .T. ) ;
#493 = VECTOR ( 'NONE', #6241, 1000.000000000000000 ) ;
#494 = SPHERICAL_SURFACE ( 'NONE', #5750, 3.000000000000000000 ) ;
#495 = CARTESIAN_POINT ( 'NONE',  ( 209.9999999999999716, 6.000000000000000000, 35.00000000000000000 ) ) ;
#496 = VERTEX_POINT ( 'NONE', #3251 ) ;
#497 = DIRECTION ( 'NONE',  ( 0.000000000000000000, 0.000000000000000000, -1.000000000000000000 ) ) ;
#498 = FACE_OUTER_BOUND ( 'NONE', #6861, .T. ) ;
#499 = CIRCLE ( 'NONE', #2964, 3.000000000000000888 ) ;
#500 = ORIENTED_EDGE ( 'NONE', *, *, #6435, .T. ) ;
#501 = EDGE_LOOP ( 'NONE', ( #4994, #7270, #5403, #348 ) ) ;
#502 = VECTOR ( 'NONE', #3666, 1000.000000000000000 ) ;
#503 = DIRECTION ( 'NONE',  ( 1.000000000000000000, 0.000000000000000000, -7.663350976776344912E-46 ) ) ;
#504 = CARTESIAN_POINT ( 'NONE',  ( 26.99871551551753868, -224.9174535703052129, 90.83998408137779279 ) ) ;
#505 = VERTEX_POINT ( 'NONE', #822 ) ;
#506 = CONTEXT_DEPENDENT_SHAPE_REPRESENTATION ( #3347, #4661 ) ;
#507 = DIRECTION ( 'NONE',  ( 0.000000000000000000, -2.065146995210485681E-16, 1.000000000000000000 ) ) ;
#508 = CARTESIAN_POINT ( 'NONE',  ( 24.99999999999999289, 86.00000000000001421, 9.999999999999992895 ) ) ;
#509 = ORIENTED_EDGE ( 'NONE', *, *, #5643, .T. ) ;
#510 = VERTEX_POINT ( 'NONE', #969 ) ;
#511 = CARTESIAN_POINT ( 'NONE',  ( 200.0000000000000000, 11.00000000000000533, -8.660254037844387298 ) ) ;
#512 = VECTOR ( 'NONE', #266, 1000.000000000000000 ) ;
#513 = ADVANCED_FACE ( 'NONE', ( #7393 ), #1436, .T. ) ;
#514 = DIRECTION ( 'NONE',  ( -1.000000000000000000, 5.551115123125783935E-17, -4.237045877651919561E-33 ) ) ;
#515 = ADVANCED_FACE ( 'NONE', ( #5022 ), #3289, .T. ) ;
#516 = CARTESIAN_POINT ( 'NONE',  ( 188.7208530678142040, 8.237612771022048364, 15.07171818587141487 ) ) ;
#517 = CYLINDRICAL_SURFACE ( 'NONE', #4229, 14.00000000000000533 ) ;
#518 = CARTESIAN_POINT ( 'NONE',  ( 10.47314606205195631, -223.0630240738404666, 96.09122589815579829 ) ) ;
#519 = DIRECTION ( 'NONE',  ( -0.4999999999999976685, 0.000000000000000000, -0.8660254037844400399 ) ) ;
#520 = CARTESIAN_POINT ( 'NONE',  ( -63.59768876112976699, -218.0630244767148440, 79.13514301043191779 ) ) ;
#521 = ORIENTED_EDGE ( 'NONE', *, *, #522, .F. ) ;
#522 = EDGE_CURVE ( 'NONE', #7372, #2111, #1110, .T. ) ;
#523 = CARTESIAN_POINT ( 'NONE',  ( 0.000000000000000000, -4.053118130421075393E-14, 7.999999999999992895 ) ) ;
#524 = FACE_OUTER_BOUND ( 'NONE', #2293, .T. ) ;
#525 = DIRECTION ( 'NONE',  ( 1.000000000000000000, 0.000000000000000000, 0.000000000000000000 ) ) ;
#526 = CARTESIAN_POINT ( 'NONE',  ( 12.50000000000000355, 101.5000000000000000, -1.214306433183764966E-14 ) ) ;
#527 = DIRECTION ( 'NONE',  ( 0.000000000000000000, 0.000000000000000000, 1.000000000000000000 ) ) ;
#528 = CIRCLE ( 'NONE', #4838, 8.500000000000007105 ) ;
#529 = VERTEX_POINT ( 'NONE', #5054 ) ;
#530 = ORIENTED_EDGE ( 'NONE', *, *, #778, .F. ) ;
#531 = CARTESIAN_POINT ( 'NONE',  ( 25.00000000000000711, 40.21320343559642652, 0.9999999999999956701 ) ) ;
#532 = CARTESIAN_POINT ( 'NONE',  ( 220.0000000000000000, -20.99999999999999645, 7.000000000000007994 ) ) ;
#533 = AXIS2_PLACEMENT_3D ( 'NONE', #1064, #5764, #3460 ) ;
#534 = EDGE_LOOP ( 'NONE', ( #5685, #2959, #6105, #5271 ) ) ;
#535 = CARTESIAN_POINT ( 'NONE',  ( 49.99999999999999289, -22.78166690339260825, 13.00000000000000888 ) ) ;
#536 = CARTESIAN_POINT ( 'NONE',  ( 3.000000000000000000, 56.99999999999999289, 3.000000000000021760 ) ) ;
#537 = ADVANCED_FACE ( 'NONE', ( #2015 ), #2125, .F. ) ;
#538 = ORIENTED_EDGE ( 'NONE', *, *, #2032, .F. ) ;
#539 = VECTOR ( 'NONE', #7469, 1000.000000000000000 ) ;
#540 = COLOUR_RGB ( '',0.7921568627450980005, 0.8196078431372548767, 0.9333333333333333481 ) ;
#541 = EDGE_LOOP ( 'NONE', ( #1499, #3109, #161 ) ) ;
#542 = CARTESIAN_POINT ( 'NONE',  ( -34.49999999999998579, 16.00000000000004263, 44.76505905230376925 ) ) ;
#543 = CARTESIAN_POINT ( 'NONE',  ( 10.43756829269602804, -222.2597742987530012, 95.94959129055985159 ) ) ;
#544 = ORIENTED_EDGE ( 'NONE', *, *, #6289, .T. ) ;
#545 = AXIS2_PLACEMENT_3D ( 'NONE', #2606, #4420, #913 ) ;
#546 = PRESENTATION_LAYER_ASSIGNMENT (  '', '', ( #1160 ) ) ;
#547 = DIRECTION ( 'NONE',  ( 0.000000000000000000, 0.000000000000000000, 1.000000000000000000 ) ) ;
#548 = AXIS2_PLACEMENT_3D ( 'NONE', #47, #5821, #4055 ) ;
#549 = CARTESIAN_POINT ( 'NONE',  ( 53.00000000000000711, 7.269317423140909676E-15, 13.00000000000000178 ) ) ;
#550 = ADVANCED_FACE ( 'NONE', ( #3363 ), #1049, .T. ) ;
#551 = VERTEX_POINT ( 'NONE', #1009 ) ;
#552 = VECTOR ( 'NONE', #4432, 1000.000000000000114 ) ;
#553 = VECTOR ( 'NONE', #1912, 1000.000000000000000 ) ;
#554 = CARTESIAN_POINT ( 'NONE',  ( -20.54184453752627348, -110.0418445375260603, 38.04184453752623085 ) ) ;
#555 = FACE_OUTER_BOUND ( 'NONE', #4424, .T. ) ;
#556 = LINE ( 'NONE', #1790, #3266 ) ;
#557 = CARTESIAN_POINT ( 'NONE',  ( 21.48772344548951452, -218.0630240738405234, 82.75416678248926416 ) ) ;
#558 = CARTESIAN_POINT ( 'NONE',  ( 217.0000000000000000, -60.00000000000000000, 10.00000000000000000 ) ) ;
#559 = CARTESIAN_POINT ( 'NONE',  ( -19.15685424949238325, -63.65685424949226245, 36.65685424949236193 ) ) ;
#560 = UNCERTAINTY_MEASURE_WITH_UNIT (LENGTH_MEASURE( 1.000000000000000082E-05 ), #5090, 'distance_accuracy_value', 'NONE');
#561 = EDGE_CURVE ( 'NONE', #1433, #7339, #6703, .T. ) ;
#562 = ORIENTED_EDGE ( 'NONE', *, *, #5673, .F. ) ;
#563 = ORIENTED_EDGE ( 'NONE', *, *, #3101, .T. ) ;
#564 = CARTESIAN_POINT ( 'NONE',  ( 50.00000000000000000, -15.08392021690038298, 15.00000000000000888 ) ) ;
#565 = CARTESIAN_POINT ( 'NONE',  ( 203.9378221735088630, -3.000000000000000000, 38.50000000000000000 ) ) ;
#566 = CARTESIAN_POINT ( 'NONE',  ( 190.3575543333202518, -6.378640834395509884, 16.48914306019513276 ) ) ;
#567 = AXIS2_PLACEMENT_3D ( 'NONE', #26, #2835, #485 ) ;
#568 = ADVANCED_FACE ( 'NONE', ( #2359 ), #5708, .T. ) ;
#569 = EDGE_LOOP ( 'NONE', ( #5849, #1454, #6085, #6733, #1062, #6851, #7395, #869, #7502, #4960, #1928, #6680, #4753, #4510, #3891, #4894, #31, #7507, #6786, #1205 ) ) ;
#570 = VERTEX_POINT ( 'NONE', #4716 ) ;
#571 = EDGE_CURVE ( 'NONE', #7349, #2238, #438, .T. ) ;
#572 = CARTESIAN_POINT ( 'NONE',  ( -30.49999999999999289, -218.0630240738404950, 71.94153218116483117 ) ) ;
#573 = AXIS2_PLACEMENT_3D ( 'NONE', #6167, #1981, #896 ) ;
#574 = DIRECTION ( 'NONE',  ( 0.000000000000000000, 0.000000000000000000, -1.000000000000000000 ) ) ;
#575 = ORIENTED_EDGE ( 'NONE', *, *, #667, .F. ) ;
#576 = CARTESIAN_POINT ( 'NONE',  ( 190.0729179104125137, -6.000000000000001776, 16.24264068711929454 ) ) ;
#577 = DIRECTION ( 'NONE',  ( -0.000000000000000000, -0.000000000000000000, 1.000000000000000000 ) ) ;
#578 = VERTEX_POINT ( 'NONE', #3521 ) ;
#579 = AXIS2_PLACEMENT_3D ( 'NONE', #7169, #4831, #3601 ) ;
#580 = VERTEX_POINT ( 'NONE', #6440 ) ;
#581 = EDGE_CURVE ( 'NONE', #2726, #3515, #6939, .T. ) ;
#582 = LINE ( 'NONE', #1735, #4476 ) ;
#583 = CARTESIAN_POINT ( 'NONE',  ( 17.66745985056437362, -212.4343899438515848, 94.21711093295448336 ) ) ;
#584 = VERTEX_POINT ( 'NONE', #7547 ) ;
#585 = EDGE_CURVE ( 'NONE', #1652, #3936, #2782, .T. ) ;
#586 = PRODUCT_CONTEXT ( 'NONE', #3644, 'mechanical' ) ;
#587 = DIRECTION ( 'NONE',  ( 1.000000000000000000, 0.000000000000000000, 0.000000000000000000 ) ) ;
#588 = CARTESIAN_POINT ( 'NONE',  ( 3.000000000000000000, -56.99999999999999289, 3.000000000000000444 ) ) ;
#589 = VERTEX_POINT ( 'NONE', #5133 ) ;
#590 = CARTESIAN_POINT ( 'NONE',  ( 21.50000000000000000, -223.0630240738404666, 96.09122589815579829 ) ) ;
#591 = EDGE_CURVE ( 'NONE', #4871, #7551, #2932, .T. ) ;
#592 = DIRECTION ( 'NONE',  ( 0.000000000000000000, 0.000000000000000000, 1.000000000000000000 ) ) ;
#593 = DIRECTION ( 'NONE',  ( -0.000000000000000000, 1.000000000000000000, 2.065146995210484941E-16 ) ) ;
#594 = CARTESIAN_POINT ( 'NONE',  ( 20.85637474134628988, -223.0630240738404098, 88.61643661315291354 ) ) ;
#595 = DIRECTION ( 'NONE',  ( 5.551115123125783935E-17, 1.000000000000000000, 5.166928274020107347E-17 ) ) ;
#596 = ADVANCED_BREP_SHAPE_REPRESENTATION ( '', ( #6264, #1914 ), #434 ) ;
#597 = VERTEX_POINT ( 'NONE', #470 ) ;
#598 = ADVANCED_FACE ( 'NONE', ( #7049 ), #1781, .F. ) ;
#599 = FILL_AREA_STYLE ('',( #6495 ) ) ;
#600 = DIRECTION ( 'NONE',  ( 4.622231866529368100E-33, -2.600005424922769496E-32, 1.000000000000000000 ) ) ;
#601 = DIRECTION ( 'NONE',  ( 0.000000000000000000, 0.000000000000000000, -1.000000000000000000 ) ) ;
#602 = CARTESIAN_POINT ( 'NONE',  ( 186.9464254547409041, 5.771749062884673265, 15.00000000000001066 ) ) ;
#603 = EDGE_CURVE ( 'NONE', #1345, #3492, #624, .T. ) ;
#604 = CARTESIAN_POINT ( 'NONE',  ( 189.0505338480733428, -3.000000000000787814, 18.71446023341851372 ) ) ;
#605 = ORIENTED_EDGE ( 'NONE', *, *, #3368, .F. ) ;
#606 = ORIENTED_EDGE ( 'NONE', *, *, #54, .F. ) ;
#607 = PLANE ( 'NONE',  #1074 ) ;
#608 = CARTESIAN_POINT ( 'NONE',  ( 4.000000000000000000, 0.000000000000000000, 0.000000000000000000 ) ) ;
#609 = EDGE_CURVE ( 'NONE', #5705, #2768, #1665, .T. ) ;
#610 = ADVANCED_FACE ( 'NONE', ( #1619 ), #6368, .T. ) ;
#611 = ORIENTED_EDGE ( 'NONE', *, *, #419, .T. ) ;
#612 = VECTOR ( 'NONE', #2712, 1000.000000000000000 ) ;
#613 = CARTESIAN_POINT ( 'NONE',  ( -70.24881022415654286, -216.1672007404107489, 77.37948953034242550 ) ) ;
#614 = CARTESIAN_POINT ( 'NONE',  ( 46.99999999999999289, -25.78715168812825453, 12.89530150989249258 ) ) ;
#615 = DIRECTION ( 'NONE',  ( 5.551115123125782702E-17, -0.7071067811865481278, 0.7071067811865469066 ) ) ;
#616 = PRODUCT_RELATED_PRODUCT_CATEGORY ( 'part', '', ( #5293 ) ) ;
#617 = ORIENTED_EDGE ( 'NONE', *, *, #6748, .T. ) ;
#618 = VECTOR ( 'NONE', #4221, 1000.000000000000000 ) ;
#619 = ORIENTED_EDGE ( 'NONE', *, *, #2332, .F. ) ;
#620 = AXIS2_PLACEMENT_3D ( 'NONE', #29, #3539, #7112 ) ;
#621 = CARTESIAN_POINT ( 'NONE',  ( 17.82928583850155135, -223.3951688904013224, 96.14979199081716388 ) ) ;
#622 = EDGE_LOOP ( 'NONE', ( #2754, #118 ) ) ;
#623 = APPLICATION_PROTOCOL_DEFINITION ( 'draft international standard', 'automotive_design', 1998, #106 ) ;
#624 = CIRCLE ( 'NONE', #1472, 13.99999999999999112 ) ;
#625 = DIRECTION ( 'NONE',  ( 0.000000000000000000, 0.000000000000000000, -1.000000000000000000 ) ) ;
#626 =( BOUNDED_CURVE ( )  B_SPLINE_CURVE ( 3, ( #3067, #2370, #1289, #3648 ),
 .UNSPECIFIED., .F., .T. ) 
 B_SPLINE_CURVE_WITH_KNOTS ( ( 4, 4 ),
 ( 3.309040732809481966, 4.712388980384687898 ),
 .UNSPECIFIED. ) 
 CURVE ( )  GEOMETRIC_REPRESENTATION_ITEM ( )  RATIONAL_B_SPLINE_CURVE ( ( 1.000000000000000000, 0.8425084105506491783, 0.8425084105506491783, 1.000000000000000000 ) ) 
 REPRESENTATION_ITEM ( '' )  );
#627 = CARTESIAN_POINT ( 'NONE',  ( -21.50000000000000000, -215.0630240738404950, 71.13768460387149162 ) ) ;
#628 = VERTEX_POINT ( 'NONE', #6978 ) ;
#629 = CIRCLE ( 'NONE', #6648, 6.000000000000003553 ) ;
#630 = DIRECTION ( 'NONE',  ( 0.000000000000000000, -1.000000000000000000, -1.221245327087672392E-15 ) ) ;
#631 = DIRECTION ( 'NONE',  ( -1.000000000000000000, 5.551115123125783935E-17, -4.237045877651919561E-33 ) ) ;
#632 =( LENGTH_UNIT ( ) NAMED_UNIT ( * ) SI_UNIT ( .MILLI., .METRE. ) );
#633 = CARTESIAN_POINT ( 'NONE',  ( 18.83797478939531445, -218.0630240738405234, 91.18492895007960897 ) ) ;
#634 = CARTESIAN_POINT ( 'NONE',  ( 53.00000000000000711, -22.78166690339260825, 13.00000000000000888 ) ) ;
#635 = CYLINDRICAL_SURFACE ( 'NONE', #1469, 3.000000000000002665 ) ;
#636 = EDGE_CURVE ( 'NONE', #1438, #2599, #1086, .T. ) ;
#637 = UNCERTAINTY_MEASURE_WITH_UNIT (LENGTH_MEASURE( 1.000000000000000082E-05 ), #5446, 'distance_accuracy_value', 'NONE');
#638 = ORIENTED_EDGE ( 'NONE', *, *, #5829, .F. ) ;
#639 = AXIS2_PLACEMENT_3D ( 'NONE', #6879, #1719, #7491 ) ;
#640 = VERTEX_POINT ( 'NONE', #1124 ) ;
#641 = DIRECTION ( 'NONE',  ( 0.000000000000000000, -1.000000000000000000, -3.304235192336776498E-16 ) ) ;
#642 = LINE ( 'NONE', #7218, #2236 ) ;
#643 = FACE_OUTER_BOUND ( 'NONE', #1378, .T. ) ;
#644 = DIRECTION ( 'NONE',  ( 0.000000000000000000, 0.000000000000000000, 1.000000000000000000 ) ) ;
#645 = DIRECTION ( 'NONE',  ( 1.000000000000000000, 0.000000000000000000, 0.000000000000000000 ) ) ;
#646 = ORIENTED_EDGE ( 'NONE', *, *, #585, .F. ) ;
#647 = VERTEX_POINT ( 'NONE', #5824 ) ;
#648 = CARTESIAN_POINT ( 'NONE',  ( 25.00000000000002842, 73.78679656440351664, 11.00000000000000178 ) ) ;
#649 = FACE_OUTER_BOUND ( 'NONE', #2456, .T. ) ;
#650 = EDGE_LOOP ( 'NONE', ( #2954, #2166, #606, #1222 ) ) ;
#651 = CARTESIAN_POINT ( 'NONE',  ( -60.72636667137881972, -221.3248423084427543, 72.81553374298034953 ) ) ;
#652 = CARTESIAN_POINT ( 'NONE',  ( -10.49999999999998224, -99.90626354475340065, 72.90626354475362803 ) ) ;
#653 = DIRECTION ( 'NONE',  ( -1.000000000000000000, 0.000000000000000000, 0.000000000000000000 ) ) ;
#654 = EDGE_LOOP ( 'NONE', ( #88, #4351, #3432, #5827 ) ) ;
#655 =( BOUNDED_CURVE ( )  B_SPLINE_CURVE ( 3, ( #4048, #6313, #6927, #1729 ),
 .UNSPECIFIED., .F., .T. ) 
 B_SPLINE_CURVE_WITH_KNOTS ( ( 4, 4 ),
 ( 1.570796326794896558, 2.443460952792054108 ),
 .UNSPECIFIED. ) 
 CURVE ( )  GEOMETRIC_REPRESENTATION_ITEM ( )  RATIONAL_B_SPLINE_CURVE ( ( 1.000000000000000000, 0.9375385246911008830, 0.9375385246911008830, 1.000000000000000000 ) ) 
 REPRESENTATION_ITEM ( '' )  );
#656 = EDGE_CURVE ( 'NONE', #7224, #7378, #6272, .T. ) ;
#657 = ORIENTED_EDGE ( 'NONE', *, *, #971, .T. ) ;
#658 = VECTOR ( 'NONE', #2207, 1000.000000000000000 ) ;
#659 = CIRCLE ( 'NONE', #1633, 10.00000000000000178 ) ;
#660 = DIRECTION ( 'NONE',  ( 0.000000000000000000, 0.000000000000000000, -1.000000000000000000 ) ) ;
#661 = CARTESIAN_POINT ( 'NONE',  ( 10.48785751550376766, -228.1620966263577657, 74.64757051591513459 ) ) ;
#662 = ORIENTED_EDGE ( 'NONE', *, *, #7419, .T. ) ;
#663 = DIRECTION ( 'NONE',  ( -1.000000000000000000, -0.000000000000000000, -0.000000000000000000 ) ) ;
#664 = DIRECTION ( 'NONE',  ( 0.000000000000000000, 0.000000000000000000, -1.000000000000000000 ) ) ;
#665 = AXIS2_PLACEMENT_3D ( 'NONE', #5893, #7160, #3594 ) ;
#666 = ORIENTED_EDGE ( 'NONE', *, *, #3367, .T. ) ;
#667 = EDGE_CURVE ( 'NONE', #5033, #5513, #2899, .T. ) ;
#668 = DIRECTION ( 'NONE',  ( 9.231085635203014490E-31, 0.000000000000000000, -1.000000000000000000 ) ) ;
#669 = AXIS2_PLACEMENT_3D ( 'NONE', #2903, #631, #1204 ) ;
#670 = DIRECTION ( 'NONE',  ( 1.000000000000000000, 0.000000000000000000, 0.000000000000000000 ) ) ;
#671 = AXIS2_PLACEMENT_3D ( 'NONE', #3826, #6742, #6159 ) ;
#672 =( BOUNDED_SURFACE ( )  B_SPLINE_SURFACE ( 3, 2, ( 
 ( #5769, #2839, #5191 ),
 ( #7528, #2269, #4622 ),
 ( #1686, #7146, #6573 ),
 ( #5996, #3657, #720 ),
 ( #4734, #2488, #4845 ),
 ( #7181, #1915, #2914 ),
 ( #566, #5269, #77 ),
 ( #4266, #5879, #1298 ),
 ( #3614, #3074, #604 ),
 ( #5729, #4158, #5421 ) ),
 .UNSPECIFIED., .F., .F., .F. ) 
 B_SPLINE_SURFACE_WITH_KNOTS ( ( 4, 2, 2, 2, 4 ),
 ( 3, 3 ),
 ( 0.000000000000000000, 0.3926990816987241395, 0.7853981633974482790, 1.178097245096172418, 1.570796326794896558 ),
 ( 0.000000000000000000, 1.000000000000000000 ),
 .UNSPECIFIED. ) 
 GEOMETRIC_REPRESENTATION_ITEM ( )  RATIONAL_B_SPLINE_SURFACE ( (
 ( 1.000000000000000000, 0.8660254037844387076, 1.000000000000000000),
 ( 1.000000000000000000, 0.8660344512784944326, 1.000000000000000000),
 ( 1.000000000000000000, 0.8622916024758332521, 1.000000000000000000),
 ( 1.000000000000000000, 0.8476439321310361708, 1.000000000000000000),
 ( 1.000000000000000000, 0.8367284556825863584, 1.000000000000000000),
 ( 1.000000000000000000, 0.8086003203334847234, 1.000000000000000000),
 ( 1.000000000000000000, 0.7913838405144675292, 1.000000000000000000),
 ( 1.000000000000000000, 0.7522104819566599598, 1.000000000000000000),
 ( 1.000000000000000000, 0.7302616374798159837, 1.000000000000000000),
 ( 1.000000000000000000, 0.7071067811865475727, 1.000000000000000000) ) ) 
 REPRESENTATION_ITEM ( '' )  SURFACE ( )  );
#673 = CARTESIAN_POINT ( 'NONE',  ( 176.5000000000000000, -39.99999999999999289, 0.000000000000000000 ) ) ;
#674 = CARTESIAN_POINT ( 'NONE',  ( 19.00163867460213396, -218.0630240738404666, 76.36460184284905495 ) ) ;
#675 = CYLINDRICAL_SURFACE ( 'NONE', #2585, 7.000000000000017764 ) ;
#676 = CARTESIAN_POINT ( 'NONE',  ( 217.0000000000000000, -3.000000000000000000, 0.000000000000000000 ) ) ;
#677 = CIRCLE ( 'NONE', #3015, 9.999999999999998224 ) ;
#678 = AXIS2_PLACEMENT_3D ( 'NONE', #4156, #3034, #3496 ) ;
#679 = DIRECTION ( 'NONE',  ( 0.000000000000000000, 0.000000000000000000, -1.000000000000000000 ) ) ;
#680 = DIRECTION ( 'NONE',  ( 0.000000000000000000, -0.000000000000000000, 1.000000000000000000 ) ) ;
#681 = CYLINDRICAL_SURFACE ( 'NONE', #5847, 6.000000000000000888 ) ;
#682 = EDGE_CURVE ( 'NONE', #797, #570, #859, .T. ) ;
#683 = DIRECTION ( 'NONE',  ( 0.000000000000000000, 0.000000000000000000, -1.000000000000000000 ) ) ;
#684 = CARTESIAN_POINT ( 'NONE',  ( 35.00000000000000000, -39.99999999999999289, 0.000000000000000000 ) ) ;
#685 = ORIENTED_EDGE ( 'NONE', *, *, #2916, .F. ) ;
#686 = CARTESIAN_POINT ( 'NONE',  ( 48.84364016120891705, -25.18505342979141304, 12.91627608905694302 ) ) ;
#687 = VERTEX_POINT ( 'NONE', #3637 ) ;
#688 = LINE ( 'NONE', #1876, #3153 ) ;
#689 = ADVANCED_FACE ( 'NONE', ( #6049 ), #4252, .T. ) ;
#690 = DIRECTION ( 'NONE',  ( 9.231085635203014490E-31, 0.000000000000000000, -1.000000000000000000 ) ) ;
#691 = ORIENTED_EDGE ( 'NONE', *, *, #5164, .T. ) ;
#692 = CARTESIAN_POINT ( 'NONE',  ( -60.81252276423130354, -227.0484711946333789, 74.34917548081020300 ) ) ;
#693 = AXIS2_PLACEMENT_3D ( 'NONE', #2604, #2683, #5730 ) ;
#694 = FACE_OUTER_BOUND ( 'NONE', #4550, .T. ) ;
#695 = CARTESIAN_POINT ( 'NONE',  ( -55.83236997523459166, -218.0620500881349528, 94.91109968007503994 ) ) ;
#696 = ORIENTED_EDGE ( 'NONE', *, *, #1553, .F. ) ;
#697 = ORIENTED_EDGE ( 'NONE', *, *, #1070, .T. ) ;
#698 = VECTOR ( 'NONE', #1441, 1000.000000000000000 ) ;
#699 = LINE ( 'NONE', #6, #2270 ) ;
#700 = CARTESIAN_POINT ( 'NONE',  ( 27.24881022415653220, -216.1672007404107205, 77.37948953034242550 ) ) ;
#701 = ORIENTED_EDGE ( 'NONE', *, *, #4267, .T. ) ;
#702 = EDGE_CURVE ( 'NONE', #3466, #1233, #6402, .T. ) ;
#703 = DIRECTION ( 'NONE',  ( -0.000000000000000000, -1.000000000000000000, -0.000000000000000000 ) ) ;
#704 = CARTESIAN_POINT ( 'NONE',  ( 37.99999999999998579, 0.000000000000000000, 1.387778780781445676E-14 ) ) ;
#705 = AXIS2_PLACEMENT_3D ( 'NONE', #885, #2584, #4943 ) ;
#706 = ORIENTED_EDGE ( 'NONE', *, *, #2708, .F. ) ;
#707 = DIRECTION ( 'NONE',  ( 5.551115123125783935E-17, 1.000000000000000000, -2.214819436045321778E-32 ) ) ;
#708 = CARTESIAN_POINT ( 'NONE',  ( -20.06899017871461410, -73.43085575620199279, 46.43085575620209227 ) ) ;
#709 = LINE ( 'NONE', #4292, #2595 ) ;
#710 = ADVANCED_FACE ( 'NONE', ( #1346 ), #771, .F. ) ;
#711 = DIRECTION ( 'NONE',  ( 1.000000000000000000, 0.000000000000000000, 0.000000000000000000 ) ) ;
#712 = DIRECTION ( 'NONE',  ( 0.000000000000000000, 0.000000000000000000, -1.000000000000000000 ) ) ;
#713 = EDGE_CURVE ( 'NONE', #5693, #4091, #1602, .T. ) ;
#714 = LINE ( 'NONE', #5337, #939 ) ;
#715 =( NAMED_UNIT ( * ) PLANE_ANGLE_UNIT ( ) SI_UNIT ( $, .RADIAN. ) );
#716 = FACE_OUTER_BOUND ( 'NONE', #6253, .T. ) ;
#717 = DIRECTION ( 'NONE',  ( 7.006492321624086910E-46, -1.221245327087672392E-15, 1.000000000000000000 ) ) ;
#718 = CARTESIAN_POINT ( 'NONE',  ( 36.00000000000000000, 0.000000000000000000, 1.387778780781445676E-14 ) ) ;
#719 = CARTESIAN_POINT ( 'NONE',  ( -21.50000000000000000, -104.1739323729103575, 75.12787131935897378 ) ) ;
#720 = CARTESIAN_POINT ( 'NONE',  ( 186.4771806038177147, -5.978286120977721829, 14.25728166854551660 ) ) ;
#721 = ORIENTED_EDGE ( 'NONE', *, *, #3201, .F. ) ;
#722 = VERTEX_POINT ( 'NONE', #4827 ) ;
#723 = CARTESIAN_POINT ( 'NONE',  ( -64.50000000000000000, -49.37258300203047412, 6.000000000000000888 ) ) ;
#724 = FACE_OUTER_BOUND ( 'NONE', #5224, .T. ) ;
#725 = DIRECTION ( 'NONE',  ( -4.622231866529368100E-33, 2.600005424922769496E-32, -1.000000000000000000 ) ) ;
#726 = FACE_BOUND ( 'NONE', #755, .T. ) ;
#727 = DIRECTION ( 'NONE',  ( 0.000000000000000000, 0.000000000000000000, 1.000000000000000000 ) ) ;
#728 = EDGE_LOOP ( 'NONE', ( #1559, #6181 ) ) ;
#729 = ADVANCED_FACE ( 'NONE', ( #2549 ), #3016, .T. ) ;
#730 = ORIENTED_EDGE ( 'NONE', *, *, #5176, .F. ) ;
#731 = AXIS2_PLACEMENT_3D ( 'NONE', #6131, #2590, #3794 ) ;
#732 = DIRECTION ( 'NONE',  ( -1.000000000000000000, 5.551115123125783935E-17, -4.237045877651919561E-33 ) ) ;
#733 = CARTESIAN_POINT ( 'NONE',  ( 27.25616595088856542, -215.8398321358105250, 77.29937933778069237 ) ) ;
#734 = VERTEX_POINT ( 'NONE', #5366 ) ;
#735 = DIRECTION ( 'NONE',  ( 1.000000000000000000, 0.000000000000000000, 0.000000000000000000 ) ) ;
#736 = DIRECTION ( 'NONE',  ( 1.000000000000000000, 1.853902270198408060E-44, 1.681558157189780485E-44 ) ) ;
#737 = CLOSED_SHELL ( 'NONE', ( #2152, #6033, #6330, #1229, #6225, #3190, #5365, #1132, #3312, #378 ) ) ;
#738 = VECTOR ( 'NONE', #5916, 1000.000000000000000 ) ;
#739 = ORIENTED_EDGE ( 'NONE', *, *, #5880, .T. ) ;
#740 = ADVANCED_FACE ( 'NONE', ( #6011 ), #6517, .F. ) ;
#741 = PLANE ( 'NONE',  #7336 ) ;
#742 = DIRECTION ( 'NONE',  ( -1.000000000000000000, -0.000000000000000000, -0.000000000000000000 ) ) ;
#743 =( LENGTH_UNIT ( ) NAMED_UNIT ( * ) SI_UNIT ( .MILLI., .METRE. ) );
#744 = CARTESIAN_POINT ( 'NONE',  ( 220.0000000000000000, 56.99999999999999289, 3.000000000000021760 ) ) ;
#745 = DIRECTION ( 'NONE',  ( -2.465190328815661892E-32, -1.000000000000000000, -1.193489751472043281E-15 ) ) ;
#746 = ORIENTED_EDGE ( 'NONE', *, *, #831, .F. ) ;
#747 = ADVANCED_FACE ( 'NONE', ( #4175 ), #2436, .F. ) ;
#748 = EDGE_CURVE ( 'NONE', #3851, #245, #1979, .T. ) ;
#749 = DIRECTION ( 'NONE',  ( 0.000000000000000000, 0.000000000000000000, 1.000000000000000000 ) ) ;
#750 = CARTESIAN_POINT ( 'NONE',  ( 35.00000000000000000, -39.99999999999999289, 10.00000000000000355 ) ) ;
#751 = DIRECTION ( 'NONE',  ( 0.000000000000000000, 0.9993908270190955401, -0.03489949670250403618 ) ) ;
#752 = CARTESIAN_POINT ( 'NONE',  ( -21.49436104581528184, -113.9621117585879944, 41.96211175858819331 ) ) ;
#753 = CARTESIAN_POINT ( 'NONE',  ( -63.79792493780531260, -223.0630240738405234, 80.77363827126067974 ) ) ;
#754 = LINE ( 'NONE', #3182, #2092 ) ;
#755 = EDGE_LOOP ( 'NONE', ( #2892, #3943 ) ) ;
#756 = EDGE_CURVE ( 'NONE', #5055, #4559, #2470, .T. ) ;
#757 = EDGE_CURVE ( 'NONE', #2650, #2663, #6890, .T. ) ;
#758 = ORIENTED_EDGE ( 'NONE', *, *, #2956, .T. ) ;
#759 = CARTESIAN_POINT ( 'NONE',  ( 24.99999999999999289, 86.00000000000001421, 0.000000000000000000 ) ) ;
#760 = AXIS2_PLACEMENT_3D ( 'NONE', #488, #6260, #527 ) ;
#761 = DIRECTION ( 'NONE',  ( -0.000000000000000000, 1.000000000000000000, 2.065146995210484941E-16 ) ) ;
#762 = CARTESIAN_POINT ( 'NONE',  ( -60.75187451922244719, -223.0194114314941203, 73.26959217102434252 ) ) ;
#763 = CARTESIAN_POINT ( 'NONE',  ( -10.49999999999997513, -104.2695387347598057, 32.26953873475996204 ) ) ;
#764 = DIRECTION ( 'NONE',  ( 0.000000000000000000, 0.000000000000000000, -1.000000000000000000 ) ) ;
#765 = ORIENTED_EDGE ( 'NONE', *, *, #757, .F. ) ;
#766 = ORIENTED_EDGE ( 'NONE', *, *, #1949, .T. ) ;
#767 = CARTESIAN_POINT ( 'NONE',  ( 50.00000000000000000, 0.000000000000000000, 35.00000000000000000 ) ) ;
#768 = CARTESIAN_POINT ( 'NONE',  ( -24.15685424949239746, 16.00000000000004263, 36.34314575050770202 ) ) ;
#769 = ORIENTED_EDGE ( 'NONE', *, *, #1167, .F. ) ;
#770 = ADVANCED_FACE ( 'NONE', ( #7163, #4901 ), #5439, .T. ) ;
#771 = CYLINDRICAL_SURFACE ( 'NONE', #6523, 8.500000000000007105 ) ;
#772 = EDGE_CURVE ( 'NONE', #7358, #5895, #5896, .T. ) ;
#773 = CARTESIAN_POINT ( 'NONE',  ( 209.9999999999999716, 6.000000000000000000, 35.00000000000000000 ) ) ;
#774 = ORIENTED_EDGE ( 'NONE', *, *, #3349, .F. ) ;
#775 = CARTESIAN_POINT ( 'NONE',  ( 27.99999999999998579, 1.224646799147344973E-15, -9.999999999999998224 ) ) ;
#776 = DIRECTION ( 'NONE',  ( 0.000000000000000000, 0.000000000000000000, 1.000000000000000000 ) ) ;
#777 = AXIS2_PLACEMENT_3D ( 'NONE', #2319, #3441, #7541 ) ;
#778 = EDGE_CURVE ( 'NONE', #4559, #722, #1243, .T. ) ;
#779 = CYLINDRICAL_SURFACE ( 'NONE', #4332, 3.000000000000000444 ) ;
#780 = CIRCLE ( 'NONE', #6074, 6.000000000000000000 ) ;
#781 = CARTESIAN_POINT ( 'NONE',  ( 35.00000000000000000, 39.99999999999999289, 10.00000000000000355 ) ) ;
#782 = DIRECTION ( 'NONE',  ( 0.000000000000000000, -1.000000000000000000, 0.000000000000000000 ) ) ;
#783 = EDGE_LOOP ( 'NONE', ( #3895, #1023, #7436, #4318 ) ) ;
#784 = ORIENTED_EDGE ( 'NONE', *, *, #962, .F. ) ;
#785 = VECTOR ( 'NONE', #6158, 1000.000000000000000 ) ;
#786=STYLED_ITEM('',(#7617),#6351);
#787 = CIRCLE ( 'NONE', #5834, 5.999999999999999112 ) ;
#788 = CARTESIAN_POINT ( 'NONE',  ( 220.0000000000000000, 9.000000000000001776, 12.00000000000000888 ) ) ;
#789 = CARTESIAN_POINT ( 'NONE',  ( -78.75983027283936622, -69.18339347973480358, -2.816606520265136027 ) ) ;
#790 = DIRECTION ( 'NONE',  ( 5.605193857299270773E-45, 0.000000000000000000, 1.000000000000000000 ) ) ;
#791 = DIRECTION ( 'NONE',  ( -0.4999999999999967804, 0.000000000000000000, -0.8660254037844405950 ) ) ;
#792 = CARTESIAN_POINT ( 'NONE',  ( -58.19347660815660817, -223.0630240738404666, 74.43406038553092685 ) ) ;
#793 = CARTESIAN_POINT ( 'NONE',  ( -21.50000000000000000, -125.0933926253236308, 30.46597562735434295 ) ) ;
#794 = AXIS2_PLACEMENT_3D ( 'NONE', #6001, #34, #5427 ) ;
#795 = ADVANCED_FACE ( 'NONE', ( #2508 ), #2973, .F. ) ;
#796 = AXIS2_PLACEMENT_3D ( 'NONE', #6678, #5607, #2529 ) ;
#797 = VERTEX_POINT ( 'NONE', #1821 ) ;
#798 = ORIENTED_EDGE ( 'NONE', *, *, #284, .F. ) ;
#799 = VECTOR ( 'NONE', #6042, 1000.000000000000000 ) ;
#800 = PRODUCT_DEFINITION_FORMATION_WITH_SPECIFIED_SOURCE ( 'ANY', '', #3413, .NOT_KNOWN. ) ;
#801 = CARTESIAN_POINT ( 'NONE',  ( 26.49999999999999645, 39.99999999999999289, 10.00000000000000355 ) ) ;
#802 = DIRECTION ( 'NONE',  ( 4.622231866529368100E-33, -2.600005424922769496E-32, 1.000000000000000000 ) ) ;
#803 = LINE ( 'NONE', #2572, #1679 ) ;
#804 = ADVANCED_FACE ( 'NONE', ( #4358 ), #3896, .F. ) ;
#805 = CARTESIAN_POINT ( 'NONE',  ( -64.08602328290328387, -218.0612840253216405, 86.88646258543963086 ) ) ;
#806 = ORIENTED_EDGE ( 'NONE', *, *, #5424, .T. ) ;
#807 = ORIENTED_EDGE ( 'NONE', *, *, #4249, .F. ) ;
#808 = CARTESIAN_POINT ( 'NONE',  ( 12.50000000000001066, 12.50000000000001066, 4.999999999999995559 ) ) ;
#809 = CARTESIAN_POINT ( 'NONE',  ( 10.01709100512437267, -217.7372475398855727, 71.85424062197864714 ) ) ;
#810 = ORIENTED_EDGE ( 'NONE', *, *, #4786, .T. ) ;
#811 = DIRECTION ( 'NONE',  ( 0.000000000000000000, 0.000000000000000000, -1.000000000000000000 ) ) ;
#812 = DIRECTION ( 'NONE',  ( 1.000000000000000000, 0.000000000000000000, 0.000000000000000000 ) ) ;
#813 = EDGE_LOOP ( 'NONE', ( #2631, #3039, #4537, #1805, #3309 ) ) ;
#814 = AXIS2_PLACEMENT_3D ( 'NONE', #5388, #2457, #3733 ) ;
#815 = ADVANCED_FACE ( 'NONE', ( #6736 ), #3707, .T. ) ;
#816 = PLANE ( 'NONE',  #1687 ) ;
#817 = DIRECTION ( 'NONE',  ( 0.000000000000000000, 0.000000000000000000, -1.000000000000000000 ) ) ;
#818 = ORIENTED_EDGE ( 'NONE', *, *, #1594, .F. ) ;
#819 = AXIS2_PLACEMENT_3D ( 'NONE', #3115, #5468, #2541 ) ;
#820 =( NAMED_UNIT ( * ) PLANE_ANGLE_UNIT ( ) SI_UNIT ( $, .RADIAN. ) );
#821 = CARTESIAN_POINT ( 'NONE',  ( 3.000000000000002665, 56.99999999999999289, 7.000000000000022204 ) ) ;
#822 = CARTESIAN_POINT ( 'NONE',  ( 1.387778780781445676E-14, 12.49999999999998401, 0.000000000000000000 ) ) ;
#823 = CARTESIAN_POINT ( 'NONE',  ( 0.000000000000000000, 0.000000000000000000, 0.000000000000000000 ) ) ;
#824 = VECTOR ( 'NONE', #7054, 999.9999999999998863 ) ;
#825 = DIRECTION ( 'NONE',  ( 0.000000000000000000, -0.9993908270190955401, 0.03489949670250346025 ) ) ;
#826 = CARTESIAN_POINT ( 'NONE',  ( 40.00000000000000000, -4.163336342344337027E-14, 1.387778780781445676E-14 ) ) ;
#827 = CARTESIAN_POINT ( 'NONE',  ( -63.60807779484393620, -223.0630240738404382, 80.31542455955738546 ) ) ;
#828 = ORIENTED_EDGE ( 'NONE', *, *, #1061, .F. ) ;
#829 = LINE ( 'NONE', #1950, #3080 ) ;
#830 = EDGE_LOOP ( 'NONE', ( #7242, #2031, #1689, #6360 ) ) ;
#831 = EDGE_CURVE ( 'NONE', #3147, #7378, #499, .T. ) ;
#832 = ORIENTED_EDGE ( 'NONE', *, *, #4232, .F. ) ;
#833 = EDGE_CURVE ( 'NONE', #7034, #6433, #7263, .T. ) ;
#834 = DIRECTION ( 'NONE',  ( -1.000000000000000000, 0.000000000000000000, 0.000000000000000000 ) ) ;
#835 = LINE ( 'NONE', #5536, #66 ) ;
#836 = CARTESIAN_POINT ( 'NONE',  ( 50.00000000000000000, -25.88825784476432545, 10.00000000000001066 ) ) ;
#837 = FACE_OUTER_BOUND ( 'NONE', #3394, .T. ) ;
#838 = ORIENTED_EDGE ( 'NONE', *, *, #4968, .T. ) ;
#839 = ORIENTED_EDGE ( 'NONE', *, *, #7076, .T. ) ;
#840 = ADVANCED_FACE ( 'NONE', ( #7275 ), #6537, .T. ) ;
#841 = EDGE_CURVE ( 'NONE', #2502, #6942, #5585, .T. ) ;
#842 = DIRECTION ( 'NONE',  ( -0.7071067811865482389, 8.659560562354926695E-17, -0.7071067811865469066 ) ) ;
#843 = CARTESIAN_POINT ( 'NONE',  ( 0.000000000000000000, 56.99999999999999289, 0.000000000000000000 ) ) ;
#844 = ORIENTED_EDGE ( 'NONE', *, *, #4014, .T. ) ;
#845 = DIRECTION ( 'NONE',  ( -2.775557561562885829E-15, 0.000000000000000000, -1.000000000000000000 ) ) ;
#846 = DIRECTION ( 'NONE',  ( -1.000000000000000000, 0.000000000000000000, 0.000000000000000000 ) ) ;
#847 = ORIENTED_EDGE ( 'NONE', *, *, #4444, .T. ) ;
#848 = CARTESIAN_POINT ( 'NONE',  ( 0.000000000000000000, 0.000000000000000000, 0.000000000000000000 ) ) ;
#849 = CARTESIAN_POINT ( 'NONE',  ( 48.57048730951211724, 29.87494558651862420, 10.00000000000000888 ) ) ;
#850 = DIRECTION ( 'NONE',  ( 0.000000000000000000, 0.000000000000000000, 1.000000000000000000 ) ) ;
#851 = ORIENTED_EDGE ( 'NONE', *, *, #1917, .F. ) ;
#852 = LINE ( 'NONE', #1941, #3097 ) ;
#853 = VECTOR ( 'NONE', #5487, 1000.000000000000000 ) ;
#854 = DIRECTION ( 'NONE',  ( -0.000000000000000000, 1.000000000000000000, 2.065146995210484941E-16 ) ) ;
#855 = CIRCLE ( 'NONE', #6519, 10.00000000000000355 ) ;
#856 = CARTESIAN_POINT ( 'NONE',  ( -26.83962456033763999, -114.3720785834763660, 42.37207858347651523 ) ) ;
#857 = EDGE_LOOP ( 'NONE', ( #2203, #6637 ) ) ;
#858 = ORIENTED_EDGE ( 'NONE', *, *, #6448, .T. ) ;
#859 = CIRCLE ( 'NONE', #6034, 2.999999999999999112 ) ;
#860 = DIRECTION ( 'NONE',  ( 1.000000000000000000, -5.551115123125783935E-17, 4.237045877651919561E-33 ) ) ;
#861 = FACE_OUTER_BOUND ( 'NONE', #6349, .T. ) ;
#862 = CARTESIAN_POINT ( 'NONE',  ( -56.86408658970942298, -223.0633023296381907, 73.89250821964630234 ) ) ;
#863 = CARTESIAN_POINT ( 'NONE',  ( 3.000000000000002665, 56.99999999999999289, 7.000000000000021316 ) ) ;
#864 = LINE ( 'NONE', #5001, #4065 ) ;
#865 = EDGE_CURVE ( 'NONE', #3936, #6541, #2469, .T. ) ;
#866 = CIRCLE ( 'NONE', #4077, 3.000000000000000888 ) ;
#867 = SHAPE_REPRESENTATION ( 'left arm', ( #1914 ), #5724 ) ;
#868 = VERTEX_POINT ( 'NONE', #385 ) ;
#869 = ORIENTED_EDGE ( 'NONE', *, *, #6458, .F. ) ;
#870 = VECTOR ( 'NONE', #5276, 1000.000000000000114 ) ;
#871 = LINE ( 'NONE', #3958, #7326 ) ;
#872 = CARTESIAN_POINT ( 'NONE',  ( 23.99999999999999289, 0.000000000000000000, -9.999999999999994671 ) ) ;
#873 = LINE ( 'NONE', #3307, #156 ) ;
#874 =( REPRESENTATION_RELATIONSHIP ('NONE','NONE', #4862, #6715 ) REPRESENTATION_RELATIONSHIP_WITH_TRANSFORMATION ( #6439 )SHAPE_REPRESENTATION_RELATIONSHIP( ) );
#875 = EDGE_CURVE ( 'NONE', #1532, #4506, #4939, .T. ) ;
#876 = ORIENTED_EDGE ( 'NONE', *, *, #2272, .T. ) ;
#877 = VERTEX_POINT ( 'NONE', #2654 ) ;
#878 = CIRCLE ( 'NONE', #3472, 10.00000000000000355 ) ;
#879 = DIRECTION ( 'NONE',  ( -1.000000000000000000, -2.465190328815661892E-32, 9.244463733058732095E-33 ) ) ;
#880 = ORIENTED_EDGE ( 'NONE', *, *, #6910, .F. ) ;
#881 = DIRECTION ( 'NONE',  ( 0.000000000000000000, 0.9860132971832693549, 0.1666666666666667684 ) ) ;
#882 = DIRECTION ( 'NONE',  ( 0.000000000000000000, 0.000000000000000000, -1.000000000000000000 ) ) ;
#883 = ADVANCED_FACE ( 'NONE', ( #2043 ), #346, .F. ) ;
#884 = ORIENTED_EDGE ( 'NONE', *, *, #7595, .T. ) ;
#885 = CARTESIAN_POINT ( 'NONE',  ( 21.50000000000000000, 0.000000000000000000, 0.000000000000000000 ) ) ;
#886 = DIRECTION ( 'NONE',  ( 1.000000000000000000, 2.465190328815661892E-32, -9.244463733058732095E-33 ) ) ;
#887 = CARTESIAN_POINT ( 'NONE',  ( 12.50000000000000355, 101.5000000000000000, 4.999999999999999112 ) ) ;
#888 = ORIENTED_EDGE ( 'NONE', *, *, #1938, .F. ) ;
#889 = DIRECTION ( 'NONE',  ( 0.000000000000000000, 0.000000000000000000, 1.000000000000000000 ) ) ;
#890 = CARTESIAN_POINT ( 'NONE',  ( -53.21539232130206898, -217.2436419687049920, 95.06511182196835819 ) ) ;
#891 = CARTESIAN_POINT ( 'NONE',  ( 220.0000000000000000, -56.99999999999999289, 0.000000000000000000 ) ) ;
#892 = FILL_AREA_STYLE ('',( #6164 ) ) ;
#893 = EDGE_CURVE ( 'NONE', #6262, #6493, #6660, .T. ) ;
#894 = ORIENTED_EDGE ( 'NONE', *, *, #5077, .F. ) ;
#895 = ORIENTED_EDGE ( 'NONE', *, *, #1028, .F. ) ;
#896 = DIRECTION ( 'NONE',  ( 0.000000000000000000, 0.000000000000000000, 1.000000000000000000 ) ) ;
#897 = AXIS2_PLACEMENT_3D ( 'NONE', #5217, #1172, #1826 ) ;
#898 = FACE_OUTER_BOUND ( 'NONE', #4231, .T. ) ;
#899 = FACE_OUTER_BOUND ( 'NONE', #4290, .T. ) ;
#900 = CARTESIAN_POINT ( 'NONE',  ( 209.9999999999999716, 3.000000000000000000, 35.00000000000000000 ) ) ;
#901 = AXIS2_PLACEMENT_3D ( 'NONE', #549, #5825, #5321 ) ;
#902 = CARTESIAN_POINT ( 'NONE',  ( -61.06900945253273960, -223.0630335581889483, 76.52804181849850806 ) ) ;
#903 = CYLINDRICAL_SURFACE ( 'NONE', #5902, 8.500000000000007105 ) ;
#904 = CARTESIAN_POINT ( 'NONE',  ( 21.50000000000000000, -49.37258300203047412, -15.99999999999998579 ) ) ;
#905 = AXIS2_PLACEMENT_3D ( 'NONE', #6934, #503, #3973 ) ;
#906 = AXIS2_PLACEMENT_3D ( 'NONE', #5187, #1254, #5338 ) ;
#907 = ORIENTED_EDGE ( 'NONE', *, *, #2968, .T. ) ;
#908 = VERTEX_POINT ( 'NONE', #5548 ) ;
#909 = EDGE_CURVE ( 'NONE', #4559, #6005, #866, .T. ) ;
#910 = CARTESIAN_POINT ( 'NONE',  ( -10.49999999999997513, -59.26953873475991230, 32.26953873476001888 ) ) ;
#911 = EDGE_CURVE ( 'NONE', #496, #5696, #4466, .T. ) ;
#912 = VECTOR ( 'NONE', #4355, 1000.000000000000000 ) ;
#913 = DIRECTION ( 'NONE',  ( -3.697785493223492838E-32, -0.9659258262890682012, 0.2588190451025208505 ) ) ;
#914 = VECTOR ( 'NONE', #6477, 1000.000000000000000 ) ;
#915 = SHAPE_REPRESENTATION ( 'base', ( #1914 ), #1662 ) ;
#916 = DIRECTION ( 'NONE',  ( -5.551115123125785167E-17, 0.7071067811865452413, -0.7071067811865499042 ) ) ;
#917 = VERTEX_POINT ( 'NONE', #6810 ) ;
#918 = VECTOR ( 'NONE', #3165, 1000.000000000000000 ) ;
#919 = CIRCLE ( 'NONE', #6946, 6.000000000000000888 ) ;
#920 = VERTEX_POINT ( 'NONE', #1492 ) ;
#921 = EDGE_CURVE ( 'NONE', #1151, #2680, #4398, .T. ) ;
#922 = CARTESIAN_POINT ( 'NONE',  ( 50.04196010845020481, -18.04196010845019060, 12.50000000000000533 ) ) ;
#923 = ORIENTED_EDGE ( 'NONE', *, *, #603, .T. ) ;
#924 = CARTESIAN_POINT ( 'NONE',  ( 7.384868508162405987E-30, 0.000000000000000000, -7.999999999999992895 ) ) ;
#925 = DIRECTION ( 'NONE',  ( 4.622231866529368100E-33, -2.600005424922769496E-32, 1.000000000000000000 ) ) ;
#926 = ORIENTED_EDGE ( 'NONE', *, *, #1410, .F. ) ;
#927 = FACE_OUTER_BOUND ( 'NONE', #4248, .T. ) ;
#928 = EDGE_CURVE ( 'NONE', #734, #6541, #3746, .T. ) ;
#929 = CYLINDRICAL_SURFACE ( 'NONE', #2510, 6.000000000000000888 ) ;
#930 = FACE_OUTER_BOUND ( 'NONE', #2463, .T. ) ;
#931 = ORIENTED_EDGE ( 'NONE', *, *, #6269, .T. ) ;
#932 = CARTESIAN_POINT ( 'NONE',  ( 210.0000000000001137, 22.49999999999996447, 34.99999999999915445 ) ) ;
#933 = DIRECTION ( 'NONE',  ( 0.000000000000000000, 0.9993908270190955401, -0.03489949670250403618 ) ) ;
#934 = CARTESIAN_POINT ( 'NONE',  ( 21.50000000000000000, 6.938893903907228378E-15, -16.00000000000001421 ) ) ;
#935 = CARTESIAN_POINT ( 'NONE',  ( -21.50000000000000000, 0.000000000000000000, 0.000000000000000000 ) ) ;
#936 = ORIENTED_EDGE ( 'NONE', *, *, #152, .F. ) ;
#937 = ORIENTED_EDGE ( 'NONE', *, *, #3868, .F. ) ;
#938 = ORIENTED_EDGE ( 'NONE', *, *, #275, .F. ) ;
#939 = VECTOR ( 'NONE', #6062, 1000.000000000000000 ) ;
#940 = DIRECTION ( 'NONE',  ( -1.000000000000000000, -4.437342591868191405E-31, 3.379803290564627108E-16 ) ) ;
#941 = EDGE_CURVE ( 'NONE', #7205, #6206, #3855, .T. ) ;
#942 = FILL_AREA_STYLE ('',( #329 ) ) ;
#943 = CARTESIAN_POINT ( 'NONE',  ( 186.9765770670147447, 7.979251100714891187, 15.12226171595996149 ) ) ;
#944 = CARTESIAN_POINT ( 'NONE',  ( -57.82488719026880375, -223.0630234060879218, 95.18029550329626431 ) ) ;
#945 = DIRECTION ( 'NONE',  ( -1.000000000000000000, -0.000000000000000000, -0.000000000000000000 ) ) ;
#946 = CARTESIAN_POINT ( 'NONE',  ( 50.00000000000000000, -24.98477067547739239, 35.87248741756260983 ) ) ;
#947 = CARTESIAN_POINT ( 'NONE',  ( -57.33489972660768075, -218.0629586075543500, 94.42960329959574040 ) ) ;
#948 = AXIS2_PLACEMENT_3D ( 'NONE', #3369, #5104, #1127 ) ;
#949 = EDGE_LOOP ( 'NONE', ( #1449, #5051, #4680, #1723 ) ) ;
#950 = ORIENTED_EDGE ( 'NONE', *, *, #7157, .F. ) ;
#951 = DIRECTION ( 'NONE',  ( 1.000000000000000000, -1.294224922628222493E-31, 1.078147950931789264E-16 ) ) ;
#952 = CYLINDRICAL_SURFACE ( 'NONE', #2411, 8.000000000000007105 ) ;
#953 = DIRECTION ( 'NONE',  ( 0.7071067811865462405, 0.000000000000000000, -0.7071067811865489050 ) ) ;
#954 = DIRECTION ( 'NONE',  ( 1.000000000000000000, 0.000000000000000000, 0.000000000000000000 ) ) ;
#955 = ORIENTED_EDGE ( 'NONE', *, *, #4014, .F. ) ;
#956 = ORIENTED_EDGE ( 'NONE', *, *, #2095, .T. ) ;
#957 =( BOUNDED_CURVE ( )  B_SPLINE_CURVE ( 3, ( #2661, #2086, #6816, #1431 ),
 .UNSPECIFIED., .F., .T. ) 
 B_SPLINE_CURVE_WITH_KNOTS ( ( 4, 4 ),
 ( 3.839724354387530791, 4.329963465791603738 ),
 .UNSPECIFIED. ) 
 CURVE ( )  GEOMETRIC_REPRESENTATION_ITEM ( )  RATIONAL_B_SPLINE_CURVE ( ( 1.000000000000000000, 0.9800722126984333649, 0.9800722126984333649, 1.000000000000000000 ) ) 
 REPRESENTATION_ITEM ( '' )  );
#958 = DIRECTION ( 'NONE',  ( 0.000000000000000000, 0.000000000000000000, 1.000000000000000000 ) ) ;
#959 = VERTEX_POINT ( 'NONE', #924 ) ;
#960 = FACE_OUTER_BOUND ( 'NONE', #2232, .T. ) ;
#961 = ADVANCED_BREP_SHAPE_REPRESENTATION ( '', ( #3747, #1914 ), #6207 ) ;
#962 = EDGE_CURVE ( 'NONE', #2663, #2650, #629, .T. ) ;
#963 = ORIENTED_EDGE ( 'NONE', *, *, #1690, .T. ) ;
#964 = CARTESIAN_POINT ( 'NONE',  ( -24.49999999999998934, 16.00000000000007105, 32.26953873476009704 ) ) ;
#965 = CARTESIAN_POINT ( 'NONE',  ( 188.0000000000000000, -10.95994505756729254, 7.000000000000017764 ) ) ;
#966 = ORIENTED_EDGE ( 'NONE', *, *, #4995, .F. ) ;
#967 = DIRECTION ( 'NONE',  ( -0.9850390035862319760, 1.651874730689321873E-30, -0.1723315450341087185 ) ) ;
#968 = CARTESIAN_POINT ( 'NONE',  ( -69.99135978879996856, -225.2480063162100521, 90.90573154067853068 ) ) ;
#969 = CARTESIAN_POINT ( 'NONE',  ( 50.00000000000000000, 21.91628335801839711, 36.91742634044857141 ) ) ;
#970 = LINE ( 'NONE', #2820, #3075 ) ;
#971 = EDGE_CURVE ( 'NONE', #5359, #6935, #5515, .T. ) ;
#972 = ORIENTED_EDGE ( 'NONE', *, *, #7431, .F. ) ;
#973 = EDGE_LOOP ( 'NONE', ( #1077, #6732, #1517, #7077 ) ) ;
#974 = CARTESIAN_POINT ( 'NONE',  ( -16.49999999999996803, 16.00000000000012079, -15.99999999999995914 ) ) ;
#975 = FILL_AREA_STYLE_COLOUR ( '', #6813 ) ;
#976 = CIRCLE ( 'NONE', #3193, 2.999999999999999112 ) ;
#977 = DIRECTION ( 'NONE',  ( 0.000000000000000000, -1.000000000000000000, -1.221245327087672392E-15 ) ) ;
#978 = FACE_OUTER_BOUND ( 'NONE', #100, .T. ) ;
#979 = CARTESIAN_POINT ( 'NONE',  ( 187.2209104841768124, -6.851359138792246561, 15.00000000000000711 ) ) ;
#980 = LINE ( 'NONE', #6833, #4423 ) ;
#981 = CARTESIAN_POINT ( 'NONE',  ( -61.13443983231169199, -218.0630240738405803, 75.38912616118008714 ) ) ;
#982 = AXIS2_PLACEMENT_3D ( 'NONE', #863, #1942, #3028 ) ;
#983 = EDGE_CURVE ( 'NONE', #5743, #7468, #3337, .T. ) ;
#984 = EDGE_CURVE ( 'NONE', #7571, #2976, #4548, .T. ) ;
#985 = AXIS2_PLACEMENT_3D ( 'NONE', #793, #6172, #3145 ) ;
#986 = ORIENTED_EDGE ( 'NONE', *, *, #3814, .F. ) ;
#987 = ORIENTED_EDGE ( 'NONE', *, *, #4853, .T. ) ;
#988 = DIRECTION ( 'NONE',  ( 0.000000000000000000, 0.000000000000000000, 1.000000000000000000 ) ) ;
#989 = FACE_OUTER_BOUND ( 'NONE', #3206, .T. ) ;
#990 = DIRECTION ( 'NONE',  ( 0.000000000000000000, 0.000000000000000000, 1.000000000000000000 ) ) ;
#991 = CARTESIAN_POINT ( 'NONE',  ( 217.0000000000000000, 9.000000000000001776, 18.00000000000001066 ) ) ;
#992 = AXIS2_PLACEMENT_3D ( 'NONE', #3172, #2091, #2589 ) ;
#993 = EDGE_CURVE ( 'NONE', #1663, #6493, #1609, .T. ) ;
#994 = ORIENTED_EDGE ( 'NONE', *, *, #1081, .T. ) ;
#995 = VECTOR ( 'NONE', #3968, 1000.000000000000000 ) ;
#996 = ORIENTED_EDGE ( 'NONE', *, *, #667, .T. ) ;
#997 = CARTESIAN_POINT ( 'NONE',  ( 217.0000000000000000, -18.04196010845019060, 12.50000000000000711 ) ) ;
#998 = ORIENTED_EDGE ( 'NONE', *, *, #2075, .F. ) ;
#999 = CARTESIAN_POINT ( 'NONE',  ( 49.62135916575813610, -24.29528608451959570, 12.94727185322461871 ) ) ;
#1000 = CYLINDRICAL_SURFACE ( 'NONE', #4251, 9.999999999999998224 ) ;
#1001 = ORIENTED_EDGE ( 'NONE', *, *, #3655, .F. ) ;
#1002 = EDGE_CURVE ( 'NONE', #2056, #3791, #7485, .T. ) ;
#1003 = DIRECTION ( 'NONE',  ( 0.000000000000000000, 1.301042606982607490E-15, -1.000000000000000000 ) ) ;
#1004 = PLANE ( 'NONE',  #5223 ) ;
#1005 = ORIENTED_EDGE ( 'NONE', *, *, #6146, .T. ) ;
#1006 = DIRECTION ( 'NONE',  ( -3.500810402197253313E-17, 1.000000000000000000, 1.176355638918515229E-16 ) ) ;
#1007 = AXIS2_PLACEMENT_3D ( 'NONE', #3889, #4927, #6222 ) ;
#1008 = CARTESIAN_POINT ( 'NONE',  ( -70.03121585365657609, -223.4569485227349048, 90.54948733812102546 ) ) ;
#1009 = CARTESIAN_POINT ( 'NONE',  ( -16.49999999999996447, -57.68629150101509850, 30.68629150101520509 ) ) ;
#1010 = FACE_OUTER_BOUND ( 'NONE', #6165, .T. ) ;
#1011 = ORIENTED_EDGE ( 'NONE', *, *, #5498, .T. ) ;
#1012 = ORIENTED_EDGE ( 'NONE', *, *, #893, .T. ) ;
#1013 = LINE ( 'NONE', #2295, #5131 ) ;
#1014 = CARTESIAN_POINT ( 'NONE',  ( 186.9059892324150383, 5.031373033403108153, 15.00000000000000888 ) ) ;
#1015 = AXIS2_PLACEMENT_3D ( 'NONE', #5249, #7129, #4136 ) ;
#1016 = CARTESIAN_POINT ( 'NONE',  ( 186.1227768564662028, 7.475225542043804516, 13.64343637173987922 ) ) ;
#1017 = DIRECTION ( 'NONE',  ( 1.000000000000000000, 2.465190328815661892E-32, -9.244463733058732095E-33 ) ) ;
#1018 = DIRECTION ( 'NONE',  ( 1.000000000000000000, 0.000000000000000000, 0.000000000000000000 ) ) ;
#1019 = DIRECTION ( 'NONE',  ( 1.000000000000000000, 0.000000000000000000, 0.000000000000000000 ) ) ;
#1020 = CARTESIAN_POINT ( 'NONE',  ( -57.57279687405196711, -218.0630326314025638, 72.90762633068793264 ) ) ;
#1021 = ORIENTED_EDGE ( 'NONE', *, *, #1002, .F. ) ;
#1022 = VECTOR ( 'NONE', #4733, 1000.000000000000000 ) ;
#1023 = ORIENTED_EDGE ( 'NONE', *, *, #7481, .F. ) ;
#1024 = DIRECTION ( 'NONE',  ( 0.000000000000000000, 0.000000000000000000, -1.000000000000000000 ) ) ;
#1025 = CARTESIAN_POINT ( 'NONE',  ( -53.25759302228803449, -223.0630240738404950, 73.28127814332044920 ) ) ;
#1026 = DIRECTION ( 'NONE',  ( -5.551115123125785167E-17, 0.7071067811865452413, -0.7071067811865499042 ) ) ;
#1027 = DIRECTION ( 'NONE',  ( 1.000000000000000000, 0.000000000000000000, 0.000000000000000000 ) ) ;
#1028 = EDGE_CURVE ( 'NONE', #5645, #3, #463, .T. ) ;
#1029 = DIRECTION ( 'NONE',  ( 2.389881825834862305E-16, 0.7071067811865465735, -0.7071067811865485719 ) ) ;
#1030 = VECTOR ( 'NONE', #6185, 1000.000000000000000 ) ;
#1031 = ORIENTED_EDGE ( 'NONE', *, *, #7385, .F. ) ;
#1032 = ORIENTED_EDGE ( 'NONE', *, *, #2447, .F. ) ;
#1033 = CIRCLE ( 'NONE', #1282, 9.999999999999994671 ) ;
#1034 = PRESENTATION_LAYER_ASSIGNMENT (  '', '', ( #177 ) ) ;
#1035 = CIRCLE ( 'NONE', #671, 8.500000000000007105 ) ;
#1036 = DIRECTION ( 'NONE',  ( -0.000000000000000000, -1.000000000000000000, -0.000000000000000000 ) ) ;
#1037 = EDGE_CURVE ( 'NONE', #4091, #6371, #5300, .T. ) ;
#1038 = ORIENTED_EDGE ( 'NONE', *, *, #1220, .F. ) ;
#1039 = CARTESIAN_POINT ( 'NONE',  ( 2.775557561562891351E-14, 86.00000000000000000, 4.999999999999999112 ) ) ;
#1040 = DIRECTION ( 'NONE',  ( 0.000000000000000000, 0.000000000000000000, 1.000000000000000000 ) ) ;
#1041 = AXIS2_PLACEMENT_3D ( 'NONE', #3695, #6142, #6073 ) ;
#1042 = VECTOR ( 'NONE', #104, 1000.000000000000000 ) ;
#1043 = VECTOR ( 'NONE', #2374, 1000.000000000000000 ) ;
#1044 = ORIENTED_EDGE ( 'NONE', *, *, #682, .F. ) ;
#1045 = CARTESIAN_POINT ( 'NONE',  ( -64.50000000000000000, -49.37258300203047412, 0.000000000000000000 ) ) ;
#1046 = ORIENTED_EDGE ( 'NONE', *, *, #1617, .F. ) ;
#1047 =( NAMED_UNIT ( * ) PLANE_ANGLE_UNIT ( ) SI_UNIT ( $, .RADIAN. ) );
#1048 = CARTESIAN_POINT ( 'NONE',  ( -60.83418965632455411, -223.7273137069676352, 96.20835808347010243 ) ) ;
#1049 = CYLINDRICAL_SURFACE ( 'NONE', #5542, 2.999999999999999112 ) ;
#1050 = CARTESIAN_POINT ( 'NONE',  ( 47.00000000000000000, -25.78715168812825098, 12.89530150989249435 ) ) ;
#1051 = ORIENTED_EDGE ( 'NONE', *, *, #7061, .F. ) ;
#1052 = VERTEX_POINT ( 'NONE', #3509 ) ;
#1053 = EDGE_CURVE ( 'NONE', #7540, #4517, #655, .T. ) ;
#1054 = CARTESIAN_POINT ( 'NONE',  ( 50.01335591787553625, 18.01335591787552559, 12.66922467357069770 ) ) ;
#1055 =( LENGTH_UNIT ( ) NAMED_UNIT ( * ) SI_UNIT ( .MILLI., .METRE. ) );
#1056 = CARTESIAN_POINT ( 'NONE',  ( 24.99999999999999289, 78.92893218813451028, 2.928932188134522274 ) ) ;
#1057 = CARTESIAN_POINT ( 'NONE',  ( -63.73162345571661547, -223.0630236663108406, 88.95209687383599828 ) ) ;
#1058 = CARTESIAN_POINT ( 'NONE',  ( 19.22919491717249940, -223.0630240738404666, 77.71142956833992343 ) ) ;
#1059 = CARTESIAN_POINT ( 'NONE',  ( -21.48215622306531003, -113.7796841263388501, 41.77968412633906325 ) ) ;
#1060 = CARTESIAN_POINT ( 'NONE',  ( -61.70062949845839029, -218.0632753655198712, 76.01051187978914925 ) ) ;
#1061 = EDGE_CURVE ( 'NONE', #1926, #6198, #4197, .T. ) ;
#1062 = ORIENTED_EDGE ( 'NONE', *, *, #2200, .F. ) ;
#1063 = ORIENTED_EDGE ( 'NONE', *, *, #522, .T. ) ;
#1064 = CARTESIAN_POINT ( 'NONE',  ( 3.000000000000002665, 56.99999999999999289, 3.000000000000021760 ) ) ;
#1065 = CARTESIAN_POINT ( 'NONE',  ( 217.0000000000000000, -20.99999999999999645, 10.00000000000000888 ) ) ;
#1066 = FACE_OUTER_BOUND ( 'NONE', #7346, .T. ) ;
#1067 = CARTESIAN_POINT ( 'NONE',  ( 186.9059892324150383, 6.000000000000000000, 15.00000000000000888 ) ) ;
#1068 = CYLINDRICAL_SURFACE ( 'NONE', #270, 6.000000000000000888 ) ;
#1069 = CIRCLE ( 'NONE', #2422, 10.00000000000000355 ) ;
#1070 = EDGE_CURVE ( 'NONE', #2618, #4037, #5197, .T. ) ;
#1071 = VERTEX_POINT ( 'NONE', #6849 ) ;
#1072 = EDGE_CURVE ( 'NONE', #1754, #228, #2592, .T. ) ;
#1073 = ORIENTED_EDGE ( 'NONE', *, *, #5268, .T. ) ;
#1074 = AXIS2_PLACEMENT_3D ( 'NONE', #7225, #4233, #3694 ) ;
#1075 = CARTESIAN_POINT ( 'NONE',  ( 24.99999999999998579, 101.4999999999999858, 4.999999999999995559 ) ) ;
#1076 = DIRECTION ( 'NONE',  ( 0.000000000000000000, -1.000000000000000000, -1.221245327087672392E-15 ) ) ;
#1077 = ORIENTED_EDGE ( 'NONE', *, *, #6155, .T. ) ;
#1078 = DIRECTION ( 'NONE',  ( 1.000000000000000000, 0.000000000000000000, 0.000000000000000000 ) ) ;
#1079 = PLANE ( 'NONE',  #2524 ) ;
#1080 = ORIENTED_EDGE ( 'NONE', *, *, #6060, .T. ) ;
#1081 = EDGE_CURVE ( 'NONE', #6577, #5363, #1856, .T. ) ;
#1082 = EDGE_CURVE ( 'NONE', #647, #1980, #1440, .T. ) ;
#1083 = CARTESIAN_POINT ( 'NONE',  ( 53.00000000000547118, 24.79732742385519018, 10.00000000000000888 ) ) ;
#1084 = ORIENTED_EDGE ( 'NONE', *, *, #3702, .T. ) ;
#1085 = SHAPE_DEFINITION_REPRESENTATION ( #1742, #6715 ) ;
#1086 = LINE ( 'NONE', #3444, #1724 ) ;
#1087 = DIRECTION ( 'NONE',  ( 0.000000000000000000, 0.000000000000000000, -1.000000000000000000 ) ) ;
#1088 = ORIENTED_EDGE ( 'NONE', *, *, #4315, .T. ) ;
#1089 = ORIENTED_EDGE ( 'NONE', *, *, #2261, .F. ) ;
#1090 = LINE ( 'NONE', #4564, #6603 ) ;
#1091 = DIRECTION ( 'NONE',  ( 1.000000000000000000, 0.000000000000000000, 0.000000000000000000 ) ) ;
#1092 = CARTESIAN_POINT ( 'NONE',  ( -10.49999999999997513, 16.00000000000006750, 32.26953873476009704 ) ) ;
#1093 = CARTESIAN_POINT ( 'NONE',  ( -64.50000000000000000, -125.0933926253236450, 30.46597562735434295 ) ) ;
#1094 = CARTESIAN_POINT ( 'NONE',  ( 11.00280363943375228, -223.0630240738404382, 73.28127814332052026 ) ) ;
#1095 = CARTESIAN_POINT ( 'NONE',  ( -21.49999999999999645, -69.31370849898463860, 42.31370849898474518 ) ) ;
#1096 = CARTESIAN_POINT ( 'NONE',  ( -64.48423350399045262, -218.0630240738404666, 82.51610664137940887 ) ) ;
#1097 = EDGE_LOOP ( 'NONE', ( #288, #435, #7329, #203, #5572, #1606 ) ) ;
#1098 = EDGE_LOOP ( 'NONE', ( #1806, #3086, #4692, #894 ) ) ;
#1099 = CIRCLE ( 'NONE', #1844, 6.000000000000000000 ) ;
#1100 = CARTESIAN_POINT ( 'NONE',  ( 2.775557561562891351E-14, 40.21320343559642652, 5.999999999999996447 ) ) ;
#1101 = DIRECTION ( 'NONE',  ( 1.000000000000000000, -0.000000000000000000, -0.000000000000000000 ) ) ;
#1102 = DIRECTION ( 'NONE',  ( 1.000000000000000000, 0.000000000000000000, 0.000000000000000000 ) ) ;
#1103 = ADVANCED_FACE ( 'NONE', ( #6393 ), #126, .F. ) ;
#1104 = DIRECTION ( 'NONE',  ( 0.000000000000000000, 5.329070518200751394E-15, -1.000000000000000000 ) ) ;
#1105 = DIRECTION ( 'NONE',  ( 1.000000000000000000, 0.000000000000000000, 7.663350976776343357E-46 ) ) ;
#1106 = CIRCLE ( 'NONE', #6024, 6.000000000000000000 ) ;
#1107 = CIRCLE ( 'NONE', #6397, 6.000000000000000000 ) ;
#1108 = EDGE_LOOP ( 'NONE', ( #3910, #701, #2410, #5551 ) ) ;
#1109 = ORIENTED_EDGE ( 'NONE', *, *, #7198, .T. ) ;
#1110 = CIRCLE ( 'NONE', #992, 7.999999999999986677 ) ;
#1111 = DIRECTION ( 'NONE',  ( -4.622231866529368100E-33, 2.600005424922769496E-32, -1.000000000000000000 ) ) ;
#1112 = ADVANCED_FACE ( 'NONE', ( #1812, #1338 ), #5392, .T. ) ;
#1113 = DIRECTION ( 'NONE',  ( 0.000000000000000000, 0.000000000000000000, -1.000000000000000000 ) ) ;
#1114 = ORIENTED_EDGE ( 'NONE', *, *, #6201, .F. ) ;
#1115 = CARTESIAN_POINT ( 'NONE',  ( 49.99999999999999289, -22.78166690339261535, 10.00000000000000888 ) ) ;
#1116 = CARTESIAN_POINT ( 'NONE',  ( 2.775557561562891351E-14, 28.00000000000002487, 9.999999999999992895 ) ) ;
#1117 = AXIS2_PLACEMENT_3D ( 'NONE', #3313, #1426, #845 ) ;
#1118 = ORIENTED_EDGE ( 'NONE', *, *, #3449, .T. ) ;
#1119 = LINE ( 'NONE', #4591, #1152 ) ;
#1120 = LINE ( 'NONE', #3555, #914 ) ;
#1121 = ORIENTED_EDGE ( 'NONE', *, *, #196, .F. ) ;
#1122 = APPLICATION_PROTOCOL_DEFINITION ( 'draft international standard', 'automotive_design', 1998, #6233 ) ;
#1123 = EDGE_CURVE ( 'NONE', #2955, #4378, #5353, .T. ) ;
#1124 = CARTESIAN_POINT ( 'NONE',  ( 0.000000000000000000, 0.000000000000000000, -7.999999999999992895 ) ) ;
#1125 = DIRECTION ( 'NONE',  ( 1.000000000000000000, 0.000000000000000000, 0.000000000000000000 ) ) ;
#1126 = ORIENTED_EDGE ( 'NONE', *, *, #4267, .F. ) ;
#1127 = DIRECTION ( 'NONE',  ( -0.7660444431189622483, 1.387778780781445984E-17, 0.6427876096865581257 ) ) ;
#1128 = VECTOR ( 'NONE', #7412, 1000.000000000000000 ) ;
#1129 = DIRECTION ( 'NONE',  ( 0.000000000000000000, 1.000000000000000000, -3.556183125752453755E-15 ) ) ;
#1130 = DIRECTION ( 'NONE',  ( -1.000000000000000000, 0.000000000000000000, -7.663350976776343357E-46 ) ) ;
#1131 = CARTESIAN_POINT ( 'NONE',  ( 14.77760111023792255, -218.0630240738404950, 73.00051268027513629 ) ) ;
#1132 = ADVANCED_FACE ( 'NONE', ( #726, #694 ), #122, .F. ) ;
#1133 = CARTESIAN_POINT ( 'NONE',  ( 14.21833974672536449, -223.0630240738404950, 74.02270760457069798 ) ) ;
#1134 = CARTESIAN_POINT ( 'NONE',  ( -21.49999999999998934, -67.16361968246707193, 40.16361968246722824 ) ) ;
#1135 = EDGE_LOOP ( 'NONE', ( #7223, #3118, #6738, #2764, #1706 ) ) ;
#1136 = SURFACE_SIDE_STYLE ('',( #6418 ) ) ;
#1137 = DIRECTION ( 'NONE',  ( 1.000000000000000000, 0.000000000000000000, 0.000000000000000000 ) ) ;
#1138 = DIRECTION ( 'NONE',  ( 0.000000000000000000, 0.000000000000000000, -1.000000000000000000 ) ) ;
#1139 = CARTESIAN_POINT ( 'NONE',  ( -64.50000000000000000, -49.37258300203047412, 0.000000000000000000 ) ) ;
#1140 = VERTEX_POINT ( 'NONE', #1307 ) ;
#1141 = EDGE_CURVE ( 'NONE', #917, #3477, #3779, .T. ) ;
#1142 = ORIENTED_EDGE ( 'NONE', *, *, #4689, .T. ) ;
#1143 = EDGE_CURVE ( 'NONE', #1669, #4326, #6150, .T. ) ;
#1144 = DIRECTION ( 'NONE',  ( 1.000000000000000000, 0.000000000000000000, 0.000000000000000000 ) ) ;
#1145 = AXIS2_PLACEMENT_3D ( 'NONE', #5159, #925, #3278 ) ;
#1146 = CARTESIAN_POINT ( 'NONE',  ( -53.40199052334469343, -221.4565245236473174, 95.80795668296072165 ) ) ;
#1147 = CIRCLE ( 'NONE', #6443, 8.500000000000007105 ) ;
#1148 = ORIENTED_EDGE ( 'NONE', *, *, #841, .T. ) ;
#1149 = DIRECTION ( 'NONE',  ( 0.000000000000000000, 0.000000000000000000, -1.000000000000000000 ) ) ;
#1150 = CARTESIAN_POINT ( 'NONE',  ( 0.000000000000000000, 0.000000000000000000, -9.999999999999994671 ) ) ;
#1151 = VERTEX_POINT ( 'NONE', #7194 ) ;
#1152 = VECTOR ( 'NONE', #732, 1000.000000000000000 ) ;
#1153 = EDGE_CURVE ( 'NONE', #2279, #4312, #4817, .T. ) ;
#1154 = AXIS2_PLACEMENT_3D ( 'NONE', #410, #6345, #5545 ) ;
#1155 = ORIENTED_EDGE ( 'NONE', *, *, #7521, .T. ) ;
#1156 = DIRECTION ( 'NONE',  ( -3.081487911019577365E-33, -1.193489751472043281E-15, 1.000000000000000000 ) ) ;
#1157 = CARTESIAN_POINT ( 'NONE',  ( 10.51728042240002914, -224.0594585235269562, 96.26692417614292197 ) ) ;
#1158 = ORIENTED_EDGE ( 'NONE', *, *, #1325, .F. ) ;
#1159 = APPLICATION_PROTOCOL_DEFINITION ( 'draft international standard', 'automotive_design', 1998, #3890 ) ;
#1160=STYLED_ITEM('',(#7624),#6388);
#1161 = CARTESIAN_POINT ( 'NONE',  ( 217.0000000000000000, 6.000000000000000000, 18.00000000000001066 ) ) ;
#1162 = VECTOR ( 'NONE', #3026, 1000.000000000000000 ) ;
#1163 = DIRECTION ( 'NONE',  ( -1.000000000000000000, 0.000000000000000000, 0.000000000000000000 ) ) ;
#1164 = VERTEX_POINT ( 'NONE', #1882 ) ;
#1165 = EDGE_CURVE ( 'NONE', #7550, #687, #4238, .T. ) ;
#1166 = VECTOR ( 'NONE', #3510, 1000.000000000000000 ) ;
#1167 = EDGE_CURVE ( 'NONE', #1151, #316, #1860, .T. ) ;
#1168 = PRODUCT_DEFINITION_FORMATION_WITH_SPECIFIED_SOURCE ( 'ANY', '', #2160, .NOT_KNOWN. ) ;
#1169 = CARTESIAN_POINT ( 'NONE',  ( 40.00000000000000000, -4.163336342344337027E-14, 8.000000000000000000 ) ) ;
#1170 = LINE ( 'NONE', #2938, #1042 ) ;
#1171 = DIRECTION ( 'NONE',  ( -5.551115123125785167E-17, 0.7071067811865469066, 0.7071067811865482389 ) ) ;
#1172 = DIRECTION ( 'NONE',  ( 1.000000000000000000, -5.551115123125783935E-17, 4.237045877651920245E-33 ) ) ;
#1173 = CARTESIAN_POINT ( 'NONE',  ( 12.10006130380613243, -223.0630240738404382, 73.39180178971804480 ) ) ;
#1174 = LINE ( 'NONE', #5259, #4802 ) ;
#1175 = PRODUCT_DEFINITION_CONTEXT ( 'detailed design', #3096, 'design' ) ;
#1176 = EDGE_CURVE ( 'NONE', #4666, #1433, #5357, .T. ) ;
#1177 = ORIENTED_EDGE ( 'NONE', *, *, #1495, .F. ) ;
#1178 = DIRECTION ( 'NONE',  ( 0.000000000000000000, 0.000000000000000000, -1.000000000000000000 ) ) ;
#1179 = CARTESIAN_POINT ( 'NONE',  ( 193.5000000000000000, -39.99999999999999289, 0.000000000000000000 ) ) ;
#1180 = CARTESIAN_POINT ( 'NONE',  ( -16.49999999999996803, -49.37258300203047412, -16.00000000000004263 ) ) ;
#1181 = CYLINDRICAL_SURFACE ( 'NONE', #620, 10.00000000000000355 ) ;
#1182 = AXIS2_PLACEMENT_3D ( 'NONE', #5188, #7524, #2266 ) ;
#1183 = EDGE_LOOP ( 'NONE', ( #3146, #1369, #7460, #5155 ) ) ;
#1184 = ORIENTED_EDGE ( 'NONE', *, *, #5395, .T. ) ;
#1185 = CARTESIAN_POINT ( 'NONE',  ( 12.50000000000000355, 101.5000000000000000, 0.000000000000000000 ) ) ;
#1186 = AXIS2_PLACEMENT_3D ( 'NONE', #2671, #940, #4954 ) ;
#1187 = DIRECTION ( 'NONE',  ( -1.000000000000000000, 0.000000000000000000, -7.663350976776343357E-46 ) ) ;
#1188 = ORIENTED_EDGE ( 'NONE', *, *, #1143, .T. ) ;
#1189 = CARTESIAN_POINT ( 'NONE',  ( -60.76462208873361703, -223.8662738488898754, 73.49650827185847390 ) ) ;
#1190 = CARTESIAN_POINT ( 'NONE',  ( 46.99999999999999289, -28.78532416918554304, 10.00000000000000533 ) ) ;
#1191 = ORIENTED_EDGE ( 'NONE', *, *, #748, .F. ) ;
#1192 = AXIS2_PLACEMENT_3D ( 'NONE', #848, #2553, #6193 ) ;
#1193 = EDGE_LOOP ( 'NONE', ( #3110, #1759, #4270, #321, #6307, #2770, #3810, #4304, #5974, #5075, #3253, #4830 ) ) ;
#1194 = DIRECTION ( 'NONE',  ( 0.000000000000000000, -1.000000000000000000, -1.221245327087672392E-15 ) ) ;
#1195 = CARTESIAN_POINT ( 'NONE',  ( 17.83909347413333890, -224.0594585235269562, 96.26692417614293618 ) ) ;
#1196 = ORIENTED_EDGE ( 'NONE', *, *, #5482, .T. ) ;
#1197 = APPLICATION_PROTOCOL_DEFINITION ( 'draft international standard', 'automotive_design', 1998, #2454 ) ;
#1198 = EDGE_CURVE ( 'NONE', #7257, #1233, #3549, .T. ) ;
#1199 = DIRECTION ( 'NONE',  ( 1.000000000000000000, 0.000000000000000000, 0.000000000000000000 ) ) ;
#1200 = DIRECTION ( 'NONE',  ( 1.681558157189779489E-44, -0.02411877311568872903, 0.9997091000803153271 ) ) ;
#1201 = ORIENTED_EDGE ( 'NONE', *, *, #2873, .T. ) ;
#1202 = MANIFOLD_SOLID_BREP ( 'Fillet3', #4556 ) ;
#1203 = CARTESIAN_POINT ( 'NONE',  ( 21.50000000000000000, -218.0630240738404382, 71.94153218116483117 ) ) ;
#1204 = DIRECTION ( 'NONE',  ( 0.000000000000000000, 0.000000000000000000, 1.000000000000000000 ) ) ;
#1205 = ORIENTED_EDGE ( 'NONE', *, *, #4052, .T. ) ;
#1206 = SHAPE_REPRESENTATION ( 'small revit', ( #1914 ), #314 ) ;
#1207 = CARTESIAN_POINT ( 'NONE',  ( 53.00000000000000711, 24.00878702352406435, 10.00000000000001066 ) ) ;
#1208 = ADVANCED_FACE ( 'NONE', ( #5540 ), #5888, .T. ) ;
#1209 = CARTESIAN_POINT ( 'NONE',  ( 19.52861056693573971, -218.0630240738404950, 90.29964924649102898 ) ) ;
#1210 = CARTESIAN_POINT ( 'NONE',  ( 15.94411230092104859, -223.0630240738404382, 94.62561961047832426 ) ) ;
#1211 = CARTESIAN_POINT ( 'NONE',  ( -18.84314575050759188, -63.34314575050751017, 36.34314575050759544 ) ) ;
#1212 = ORIENTED_EDGE ( 'NONE', *, *, #4305, .T. ) ;
#1213 = ORIENTED_EDGE ( 'NONE', *, *, #6472, .F. ) ;
#1214 = LINE ( 'NONE', #5910, #5739 ) ;
#1215 = FACE_OUTER_BOUND ( 'NONE', #6173, .T. ) ;
#1216 = CARTESIAN_POINT ( 'NONE',  ( 220.0000000000000000, -18.00000000000000000, 10.00000000000000888 ) ) ;
#1217 = DIRECTION ( 'NONE',  ( 0.000000000000000000, -0.000000000000000000, -1.000000000000000000 ) ) ;
#1218 = CARTESIAN_POINT ( 'NONE',  ( 0.000000000000000000, 30.03170604878415162, 13.00000000000001066 ) ) ;
#1219 = FACE_OUTER_BOUND ( 'NONE', #2393, .T. ) ;
#1220 = EDGE_CURVE ( 'NONE', #2238, #5445, #803, .T. ) ;
#1221 = EDGE_LOOP ( 'NONE', ( #3013, #2785, #6919, #6312, #4124 ) ) ;
#1222 = ORIENTED_EDGE ( 'NONE', *, *, #2363, .F. ) ;
#1223 = CARTESIAN_POINT ( 'NONE',  ( 188.6380400399839061, -9.000000000000001776, 15.00000000000000888 ) ) ;
#1224 = LINE ( 'NONE', #3583, #5091 ) ;
#1225 = AXIS2_PLACEMENT_3D ( 'NONE', #2444, #174, #7102 ) ;
#1226 = VERTEX_POINT ( 'NONE', #6115 ) ;
#1227 = CIRCLE ( 'NONE', #5532, 23.99999999999999289 ) ;
#1228 = CARTESIAN_POINT ( 'NONE',  ( -70.21559789597881718, -215.1711607728661022, 88.90143116695425363 ) ) ;
#1229 = ADVANCED_FACE ( 'NONE', ( #837 ), #5505, .T. ) ;
#1230 = CARTESIAN_POINT ( 'NONE',  ( 3.000000000000002665, -56.99999999999999289, 10.00000000000000000 ) ) ;
#1231 = VERTEX_POINT ( 'NONE', #267 ) ;
#1232 = AXIS2_PLACEMENT_3D ( 'NONE', #447, #6214, #3375 ) ;
#1233 = VERTEX_POINT ( 'NONE', #2608 ) ;
#1234 = CARTESIAN_POINT ( 'NONE',  ( 0.000000000000000000, -56.99999999999999289, 7.000000000000000888 ) ) ;
#1235 = CARTESIAN_POINT ( 'NONE',  ( 26.99135978879997566, -225.2480063162099952, 90.90573154067851647 ) ) ;
#1236 = EDGE_LOOP ( 'NONE', ( #3768, #6263, #4015, #282, #7066, #1569, #1565, #730, #774, #4230 ) ) ;
#1237 = SHAPE_DEFINITION_REPRESENTATION ( #6357, #97 ) ;
#1238 = AXIS2_PLACEMENT_3D ( 'NONE', #4836, #4909, #1903 ) ;
#1239 = CARTESIAN_POINT ( 'NONE',  ( 26.00000000000000000, 0.000000000000000000, 0.000000000000000000 ) ) ;
#1240 = CARTESIAN_POINT ( 'NONE',  ( -13.49999999999999822, -223.0630240738404382, 73.28127814332047762 ) ) ;
#1241 = VERTEX_POINT ( 'NONE', #199 ) ;
#1242 = ADVANCED_FACE ( 'NONE', ( #4965 ), #2038, .F. ) ;
#1243 = CIRCLE ( 'NONE', #5547, 2.999999999999999112 ) ;
#1244 = DIRECTION ( 'NONE',  ( -8.758115402030108249E-46, -0.1736481776669305255, -0.9848077530122081313 ) ) ;
#1245 = LINE ( 'NONE', #3025, #5956 ) ;
#1246 =( LENGTH_UNIT ( ) NAMED_UNIT ( * ) SI_UNIT ( .MILLI., .METRE. ) );
#1247 = AXIS2_PLACEMENT_3D ( 'NONE', #6677, #5912, #113 ) ;
#1248 = CARTESIAN_POINT ( 'NONE',  ( 18.18549846063790909, -218.0630240738405519, 91.87109893316912235 ) ) ;
#1249 = CARTESIAN_POINT ( 'NONE',  ( 217.0000000000000000, 60.00000000000000000, 10.00000000000002309 ) ) ;
#1250 = CARTESIAN_POINT ( 'NONE',  ( 4.000000000000003553, 1.224646799147353059E-15, -9.999999999999984013 ) ) ;
#1251 = UNCERTAINTY_MEASURE_WITH_UNIT (LENGTH_MEASURE( 1.000000000000000082E-05 ), #4876, 'distance_accuracy_value', 'NONE');
#1252 = AXIS2_PLACEMENT_3D ( 'NONE', #6002, #725, #4854 ) ;
#1253 = CARTESIAN_POINT ( 'NONE',  ( -64.50000000000000000, -223.0630240738404950, 96.09122589815579829 ) ) ;
#1254 = DIRECTION ( 'NONE',  ( 1.000000000000000000, 1.853902270198408060E-44, -1.681558157189779738E-44 ) ) ;
#1255 = FACE_OUTER_BOUND ( 'NONE', #4425, .T. ) ;
#1256 = CYLINDRICAL_SURFACE ( 'NONE', #1292, 6.000000000000000888 ) ;
#1257 = CARTESIAN_POINT ( 'NONE',  ( 10.25168462842736261, -218.0630240738404950, 95.20959099461346398 ) ) ;
#1258 = DIRECTION ( 'NONE',  ( 1.000000000000000000, 2.465190328815661892E-32, -9.244463733058732095E-33 ) ) ;
#1259 = VERTEX_POINT ( 'NONE', #3154 ) ;
#1260 = ORIENTED_EDGE ( 'NONE', *, *, #3630, .F. ) ;
#1261 = ADVANCED_FACE ( 'NONE', ( #7108 ), #6604, .T. ) ;
#1262 = FACE_OUTER_BOUND ( 'NONE', #6520, .T. ) ;
#1263 = CARTESIAN_POINT ( 'NONE',  ( -29.64230087749237086, -110.3978942797115650, 38.39789427971174263 ) ) ;
#1264 = ORIENTED_EDGE ( 'NONE', *, *, #7048, .T. ) ;
#1265 = CARTESIAN_POINT ( 'NONE',  ( -53.33013951010422460, -224.6695236240153122, 73.71173840043080361 ) ) ;
#1266 = CARTESIAN_POINT ( 'NONE',  ( -10.49999999999998224, -106.6736682753135739, 34.67366827531366624 ) ) ;
#1267 = CARTESIAN_POINT ( 'NONE',  ( -56.20284895707440143, -218.0622243524431667, 94.81566216203397346 ) ) ;
#1268 = ORIENTED_EDGE ( 'NONE', *, *, #7247, .T. ) ;
#1269 = VERTEX_POINT ( 'NONE', #1359 ) ;
#1270 = APPLICATION_CONTEXT ( 'automotive_design' ) ;
#1271 = ADVANCED_FACE ( 'NONE', ( #2483 ), #110, .F. ) ;
#1272 = CARTESIAN_POINT ( 'NONE',  ( 2.775557561562891351E-14, 40.21320343559642652, 0.9999999999999956701 ) ) ;
#1273 = CARTESIAN_POINT ( 'NONE',  ( 10.10580595754474764, -219.7017882839730873, 72.38063772785488936 ) ) ;
#1274 = ORIENTED_EDGE ( 'NONE', *, *, #2007, .F. ) ;
#1275 = EDGE_CURVE ( 'NONE', #3543, #5645, #714, .T. ) ;
#1276 = CARTESIAN_POINT ( 'NONE',  ( 220.0000000000000000, 18.04196010845019060, 12.50000000000000711 ) ) ;
#1277 = FACE_OUTER_BOUND ( 'NONE', #2513, .T. ) ;
#1278 = AXIS2_PLACEMENT_3D ( 'NONE', #3049, #5641, #764 ) ;
#1279 =( GEOMETRIC_REPRESENTATION_CONTEXT ( 3 ) GLOBAL_UNCERTAINTY_ASSIGNED_CONTEXT ( ( #5800 ) ) GLOBAL_UNIT_ASSIGNED_CONTEXT ( ( #6568, #4693, #4223 ) ) REPRESENTATION_CONTEXT ( 'NONE', 'WORKASPACE' ) );
#1280 = ORIENTED_EDGE ( 'NONE', *, *, #5374, .F. ) ;
#1281 = PLANE ( 'NONE',  #6973 ) ;
#1282 = AXIS2_PLACEMENT_3D ( 'NONE', #4509, #7464, #2769 ) ;
#1283 = CIRCLE ( 'NONE', #669, 4.999999999999999112 ) ;
#1284 = CARTESIAN_POINT ( 'NONE',  ( 21.50000000000000000, -49.37258300203045280, -2.775557561562891351E-14 ) ) ;
#1285 = AXIS2_PLACEMENT_3D ( 'NONE', #3678, #6666, #6094 ) ;
#1286 = CARTESIAN_POINT ( 'NONE',  ( -19.15685424949238680, -108.6568542494921701, 36.65685424949233351 ) ) ;
#1287 = CARTESIAN_POINT ( 'NONE',  ( -27.57070108872857617, -112.5545107178312350, 40.55451071783139128 ) ) ;
#1288 = CARTESIAN_POINT ( 'NONE',  ( 176.5000000000000000, 39.99999999999999289, 10.00000000000000355 ) ) ;
#1289 = CARTESIAN_POINT ( 'NONE',  ( 51.46767767233085067, 19.46767767233084712, 10.00000000000001066 ) ) ;
#1290 = AXIS2_PLACEMENT_3D ( 'NONE', #5768, #2837, #6960 ) ;
#1291 = AXIS2_PLACEMENT_3D ( 'NONE', #2963, #2849, #4049 ) ;
#1292 = AXIS2_PLACEMENT_3D ( 'NONE', #718, #3612, #7143 ) ;
#1293 = ORIENTED_EDGE ( 'NONE', *, *, #6624, .F. ) ;
#1294 = FACE_OUTER_BOUND ( 'NONE', #3045, .T. ) ;
#1295 = CARTESIAN_POINT ( 'NONE',  ( -26.49999999999999289, -214.0630240738404382, 71.94153218116485959 ) ) ;
#1296 = CARTESIAN_POINT ( 'NONE',  ( 27.99999999999998579, -7.873646488999802468E-30, 9.999999999999998224 ) ) ;
#1297 = CARTESIAN_POINT ( 'NONE',  ( 23.99999999999999289, 0.000000000000000000, -3.000000000000002665 ) ) ;
#1298 = CARTESIAN_POINT ( 'NONE',  ( 188.5973441732890308, -3.156163941073441226, 17.92951269122647062 ) ) ;
#1299 = ADVANCED_FACE ( 'NONE', ( #6640 ), #3569, .F. ) ;
#1300 = ORIENTED_EDGE ( 'NONE', *, *, #9, .T. ) ;
#1301 = EDGE_LOOP ( 'NONE', ( #1300, #706, #3023, #6757 ) ) ;
#1302 = CARTESIAN_POINT ( 'NONE',  ( 0.000000000000000000, 35.07106781186547551, 2.928932188134524051 ) ) ;
#1303 = CARTESIAN_POINT ( 'NONE',  ( -53.25168462842736261, -218.0630240738404950, 95.20959099461346398 ) ) ;
#1304 = CARTESIAN_POINT ( 'NONE',  ( -53.21539232130207608, -222.1285142276788065, 73.03087698472252498 ) ) ;
#1305 = AXIS2_PLACEMENT_3D ( 'NONE', #6613, #155, #2493 ) ;
#1306 = EDGE_CURVE ( 'NONE', #2624, #4861, #6843, .T. ) ;
#1307 = CARTESIAN_POINT ( 'NONE',  ( 3.000000000000002665, 56.99999999999999289, 2.149255132503604690E-14 ) ) ;
#1308 = CARTESIAN_POINT ( 'NONE',  ( -63.70092059630563597, -218.0630238739302627, 87.96661164443882797 ) ) ;
#1309 = ORIENTED_EDGE ( 'NONE', *, *, #1788, .F. ) ;
#1310 = VERTEX_POINT ( 'NONE', #788 ) ;
#1311 = VECTOR ( 'NONE', #6828, 1000.000000000000000 ) ;
#1312 = DIRECTION ( 'NONE',  ( 0.000000000000000000, -1.000000000000000000, -0.000000000000000000 ) ) ;
#1313 = CARTESIAN_POINT ( 'NONE',  ( 17.66745985056476798, -217.4114710059388926, 71.76694906279428210 ) ) ;
#1314 = ORIENTED_EDGE ( 'NONE', *, *, #3233, .F. ) ;
#1315 = DIRECTION ( 'NONE',  ( 0.000000000000000000, -1.000000000000000000, 0.000000000000000000 ) ) ;
#1316 = CARTESIAN_POINT ( 'NONE',  ( -34.49999999999998579, -218.0630240738404382, 44.76505905230349214 ) ) ;
#1317 = EDGE_CURVE ( 'NONE', #1140, #496, #5984, .T. ) ;
#1318 = ADVANCED_FACE ( 'NONE', ( #1294 ), #4222, .T. ) ;
#1319 = ORIENTED_EDGE ( 'NONE', *, *, #5713, .T. ) ;
#1320 = DIRECTION ( 'NONE',  ( 1.000000000000000000, 2.624548829666596385E-30, 9.231085635203014490E-31 ) ) ;
#1321 = CYLINDRICAL_SURFACE ( 'NONE', #2019, 26.99999999999999289 ) ;
#1322 = ORIENTED_EDGE ( 'NONE', *, *, #7568, .T. ) ;
#1323 = FACE_OUTER_BOUND ( 'NONE', #6585, .T. ) ;
#1324 = SURFACE_STYLE_FILL_AREA ( #892 ) ;
#1325 = EDGE_CURVE ( 'NONE', #5705, #6764, #1910, .T. ) ;
#1326 = CARTESIAN_POINT ( 'NONE',  ( 170.0000000000000000, -11.00000000000000355, 8.660254037844387298 ) ) ;
#1327 = DIRECTION ( 'NONE',  ( -1.000000000000000000, -1.853902270198408060E-44, -1.681558157189780485E-44 ) ) ;
#1328 = DIRECTION ( 'NONE',  ( 1.000000000000000000, 0.000000000000000000, 0.000000000000000000 ) ) ;
#1329 = CARTESIAN_POINT ( 'NONE',  ( 25.00000000000002132, 36.67766952966366745, 4.535533905932717325 ) ) ;
#1330 = CARTESIAN_POINT ( 'NONE',  ( -63.60391380032690023, -223.0630241410106578, 80.30539155062909629 ) ) ;
#1331 = DIRECTION ( 'NONE',  ( -1.681558157189779738E-44, 0.000000000000000000, -1.000000000000000000 ) ) ;
#1332 = ORIENTED_EDGE ( 'NONE', *, *, #3954, .T. ) ;
#1333 = ORIENTED_EDGE ( 'NONE', *, *, #2440, .T. ) ;
#1334 = ADVANCED_FACE ( 'NONE', ( #4880 ), #4803, .F. ) ;
#1335 = LINE ( 'NONE', #7264, #6348 ) ;
#1336 = DIRECTION ( 'NONE',  ( 0.000000000000000000, -0.9961946980917452121, -0.08715574274766277330 ) ) ;
#1337 = CARTESIAN_POINT ( 'NONE',  ( -53.40199052334512686, -226.2606222968797169, 74.13807200490302307 ) ) ;
#1338 = FACE_BOUND ( 'NONE', #2294, .T. ) ;
#1339 = CARTESIAN_POINT ( 'NONE',  ( -64.45762304774287088, -218.0620869872676622, 84.71565845322002986 ) ) ;
#1340 = ORIENTED_EDGE ( 'NONE', *, *, #6213, .F. ) ;
#1341 = EDGE_LOOP ( 'NONE', ( #3669, #5770, #2012, #1859 ) ) ;
#1342 = EDGE_CURVE ( 'NONE', #2172, #3560, #2372, .T. ) ;
#1343 = LINE ( 'NONE', #2391, #7296 ) ;
#1344 = LINE ( 'NONE', #5476, #5709 ) ;
#1345 = VERTEX_POINT ( 'NONE', #5990 ) ;
#1346 = FACE_OUTER_BOUND ( 'NONE', #6166, .T. ) ;
#1347 = DIRECTION ( 'NONE',  ( 0.000000000000000000, 0.000000000000000000, 1.000000000000000000 ) ) ;
#1348 = AXIS2_PLACEMENT_3D ( 'NONE', #2791, #2179, #7293 ) ;
#1349 = ORIENTED_EDGE ( 'NONE', *, *, #2802, .T. ) ;
#1350 = CARTESIAN_POINT ( 'NONE',  ( 189.5040654437683258, 3.000000000000000000, 19.50000000000000711 ) ) ;
#1351 = VECTOR ( 'NONE', #7324, 1000.000000000000000 ) ;
#1352 = EDGE_CURVE ( 'NONE', #2966, #5372, #6482, .T. ) ;
#1353 = CARTESIAN_POINT ( 'NONE',  ( 3.000000000000002665, 0.000000000000000000, 60.00000000000000711 ) ) ;
#1354 = ORIENTED_EDGE ( 'NONE', *, *, #7198, .F. ) ;
#1355 =( NAMED_UNIT ( * ) PLANE_ANGLE_UNIT ( ) SI_UNIT ( $, .RADIAN. ) );
#1356 = DIRECTION ( 'NONE',  ( 0.000000000000000000, 0.08715574274766212104, -0.9961946980917452121 ) ) ;
#1357 = DIRECTION ( 'NONE',  ( 0.000000000000000000, 0.000000000000000000, -1.000000000000000000 ) ) ;
#1358 = ORIENTED_EDGE ( 'NONE', *, *, #4951, .F. ) ;
#1359 = CARTESIAN_POINT ( 'NONE',  ( -14.00000000000000000, 1.714505518806294046E-15, -39.99999999999997868 ) ) ;
#1360 = EDGE_CURVE ( 'NONE', #4415, #6542, #7573, .T. ) ;
#1361 = EDGE_CURVE ( 'NONE', #5964, #3162, #7140, .T. ) ;
#1362 =( NAMED_UNIT ( * ) SI_UNIT ( $, .STERADIAN. ) SOLID_ANGLE_UNIT ( ) );
#1363 = DIRECTION ( 'NONE',  ( 0.000000000000000000, 0.000000000000000000, -1.000000000000000000 ) ) ;
#1364 = CARTESIAN_POINT ( 'NONE',  ( -16.50000000000001066, 15.99999999999998579, 96.09122589815608251 ) ) ;
#1365 = CARTESIAN_POINT ( 'NONE',  ( -57.26052226718441318, -223.0630848540440923, 74.04027840652977943 ) ) ;
#1366 = CARTESIAN_POINT ( 'NONE',  ( 186.9059892324150383, -5.031373033403107264, 15.00000000000000888 ) ) ;
#1367 = CIRCLE ( 'NONE', #4942, 3.000000000000000000 ) ;
#1368 = ORIENTED_EDGE ( 'NONE', *, *, #1275, .T. ) ;
#1369 = ORIENTED_EDGE ( 'NONE', *, *, #7147, .F. ) ;
#1370 = LINE ( 'NONE', #723, #4017 ) ;
#1371 = CIRCLE ( 'NONE', #1252, 12.49999999999999645 ) ;
#1372 = CARTESIAN_POINT ( 'NONE',  ( 217.0000000000000000, 20.99999999999999645, 13.00000000000000888 ) ) ;
#1373 = CARTESIAN_POINT ( 'NONE',  ( 216.9999999999999716, -6.000000000000000000, 35.00000000000000000 ) ) ;
#1374 =( LENGTH_UNIT ( ) NAMED_UNIT ( * ) SI_UNIT ( .MILLI., .METRE. ) );
#1375 = CARTESIAN_POINT ( 'NONE',  ( -61.19496864977951134, -218.0630138500335704, 91.85947964960436707 ) ) ;
#1376 = EDGE_CURVE ( 'NONE', #5743, #6273, #1214, .T. ) ;
#1377 = VERTEX_POINT ( 'NONE', #2987 ) ;
#1378 = EDGE_LOOP ( 'NONE', ( #1607, #2418, #1118, #798 ) ) ;
#1379 = CARTESIAN_POINT ( 'NONE',  ( -25.67719663180530176, -106.8228033681944993, 34.82280336819465560 ) ) ;
#1380 = CARTESIAN_POINT ( 'NONE',  ( 17.80066350777958917, -226.2606222968801433, 74.13807200489549132 ) ) ;
#1381 = VERTEX_POINT ( 'NONE', #2412 ) ;
#1382 = CARTESIAN_POINT ( 'NONE',  ( 49.99999999999998579, -20.99999999999999645, 10.00000000000000888 ) ) ;
#1383 = LINE ( 'NONE', #3748, #3879 ) ;
#1384 = ORIENTED_EDGE ( 'NONE', *, *, #3640, .T. ) ;
#1385 = AXIS2_PLACEMENT_3D ( 'NONE', #2667, #5669, #471 ) ;
#1386 = CARTESIAN_POINT ( 'NONE',  ( 50.00000000000000000, 1.714505518806293455E-15, 21.00000000000001066 ) ) ;
#1387 = CARTESIAN_POINT ( 'NONE',  ( 48.75735931288071612, 27.04312195450891565, 12.73853277175702381 ) ) ;
#1388 = ORIENTED_EDGE ( 'NONE', *, *, #6838, .F. ) ;
#1389 = SHAPE_REPRESENTATION_RELATIONSHIP ( 'NONE' , 'NONE' ,  #6475, #5100 ) ;
#1390 = AXIS2_PLACEMENT_3D ( 'NONE', #4789, #5398, #7123 ) ;
#1391 = CYLINDRICAL_SURFACE ( 'NONE', #2109, 3.000000000000000000 ) ;
#1392 = AXIS2_PLACEMENT_3D ( 'NONE', #2376, #2452, #3613 ) ;
#1393 = CARTESIAN_POINT ( 'NONE',  ( -26.49999999999998934, -223.0630240738404950, 96.09122589815579829 ) ) ;
#1394 = CYLINDRICAL_SURFACE ( 'NONE', #731, 6.000000000000000000 ) ;
#1395 = ADVANCED_FACE ( 'NONE', ( #6567 ), #5416, .T. ) ;
#1396 = EDGE_CURVE ( 'NONE', #2714, #6636, #7330, .T. ) ;
#1397 = VERTEX_POINT ( 'NONE', #7398 ) ;
#1398 = VECTOR ( 'NONE', #6177, 1000.000000000000000 ) ;
#1399 = AXIS2_PLACEMENT_3D ( 'NONE', #5362, #3634, #5973 ) ;
#1400 = DIRECTION ( 'NONE',  ( -0.000000000000000000, 0.03489949670250429292, 0.9993908270190956511 ) ) ;
#1401 = SURFACE_SIDE_STYLE ('',( #5991 ) ) ;
#1402 = PLANE ( 'NONE',  #1247 ) ;
#1403 = CARTESIAN_POINT ( 'NONE',  ( 25.00000000000000711, 28.00000000000002487, 4.999999999999995559 ) ) ;
#1404 = CARTESIAN_POINT ( 'NONE',  ( -16.50000000000000000, -105.5631177942458265, 67.24940929526127320 ) ) ;
#1405 = EDGE_LOOP ( 'NONE', ( #7002, #847, #4554, #7311 ) ) ;
#1406 = DIRECTION ( 'NONE',  ( -1.681558157189779738E-44, 0.000000000000000000, -1.000000000000000000 ) ) ;
#1407 = AXIS2_PLACEMENT_3D ( 'NONE', #3227, #3808, #1336 ) ;
#1408 = MECHANICAL_DESIGN_GEOMETRIC_PRESENTATION_REPRESENTATION (  '', ( #1160 ), #302 ) ;
#1409 =( BOUNDED_CURVE ( )  B_SPLINE_CURVE ( 3, ( #7226, #6761, #4307, #5503 ),
 .UNSPECIFIED., .F., .T. ) 
 B_SPLINE_CURVE_WITH_KNOTS ( ( 4, 4 ),
 ( 1.637599047967247534, 2.356194490192342172 ),
 .UNSPECIFIED. ) 
 CURVE ( )  GEOMETRIC_REPRESENTATION_ITEM ( )  RATIONAL_B_SPLINE_CURVE ( ( 1.000000000000000000, 0.9574293250827445867, 0.9574293250827445867, 1.000000000000000000 ) ) 
 REPRESENTATION_ITEM ( '' )  );
#1410 = EDGE_CURVE ( 'NONE', #3211, #7034, #5635, .T. ) ;
#1411 = ADVANCED_FACE ( 'NONE', ( #3873, #5604 ), #6100, .T. ) ;
#1412 = ORIENTED_EDGE ( 'NONE', *, *, #1975, .F. ) ;
#1413 = VERTEX_POINT ( 'NONE', #2594 ) ;
#1414 = PRODUCT_DEFINITION ( 'UNKNOWN', '', #76, #2409 ) ;
#1415 = CIRCLE ( 'NONE', #1145, 12.49999999999999645 ) ;
#1416 = CARTESIAN_POINT ( 'NONE',  ( -21.50000000000000000, -99.90626354475344328, 72.90626354475362803 ) ) ;
#1417 = DIRECTION ( 'NONE',  ( 1.000000000000000000, 1.853902270198408060E-44, 1.681558157189780485E-44 ) ) ;
#1418 = DIRECTION ( 'NONE',  ( 0.000000000000000000, -1.000000000000000000, -1.221245327087672392E-15 ) ) ;
#1419 = CARTESIAN_POINT ( 'NONE',  ( -56.93191179421732073, -218.0627243648279716, 94.58151066868406076 ) ) ;
#1420 = EDGE_LOOP ( 'NONE', ( #7359, #3970 ) ) ;
#1421 = VERTEX_POINT ( 'NONE', #5059 ) ;
#1422 = VECTOR ( 'NONE', #1101, 1000.000000000000000 ) ;
#1423 = CARTESIAN_POINT ( 'NONE',  ( 40.00000000000000000, -4.065364598412548908E-14, -7.999999999999972466 ) ) ;
#1424 = CARTESIAN_POINT ( 'NONE',  ( 10.00237955168408632, -217.4114710059382958, 71.76694906279443842 ) ) ;
#1425 = ORIENTED_EDGE ( 'NONE', *, *, #4295, .F. ) ;
#1426 = DIRECTION ( 'NONE',  ( -0.000000000000000000, 1.000000000000000000, 0.000000000000000000 ) ) ;
#1427 = EDGE_LOOP ( 'NONE', ( #2871, #966 ) ) ;
#1428 = AXIS2_PLACEMENT_3D ( 'NONE', #5378, #2449, #3651 ) ;
#1429 = CARTESIAN_POINT ( 'NONE',  ( 21.50000000000000000, -120.9522879036832848, 45.92078884797942351 ) ) ;
#1430 = EDGE_CURVE ( 'NONE', #640, #6268, #2046, .T. ) ;
#1431 = CARTESIAN_POINT ( 'NONE',  ( -15.92209785380265608, -113.7796841263388501, 41.77968412633906325 ) ) ;
#1432 = CARTESIAN_POINT ( 'NONE',  ( 35.00000000000000000, 39.99999999999999289, 0.000000000000000000 ) ) ;
#1433 = VERTEX_POINT ( 'NONE', #6717 ) ;
#1434 = EDGE_CURVE ( 'NONE', #5929, #1595, #3281, .T. ) ;
#1435 = CARTESIAN_POINT ( 'NONE',  ( 50.00000000000000000, 0.000000000000000000, 35.00000000000000000 ) ) ;
#1436 = CYLINDRICAL_SURFACE ( 'NONE', #5660, 8.000000000000014211 ) ;
#1437 = CARTESIAN_POINT ( 'NONE',  ( 220.0000000000000000, 3.000000000000000000, 18.00000000000001066 ) ) ;
#1438 = VERTEX_POINT ( 'NONE', #6787 ) ;
#1439 = ORIENTED_EDGE ( 'NONE', *, *, #6492, .T. ) ;
#1440 =( BOUNDED_CURVE ( )  B_SPLINE_CURVE ( 3, ( #1653, #576, #4011, #3356 ),
 .UNSPECIFIED., .F., .T. ) 
 B_SPLINE_CURVE_WITH_KNOTS ( ( 4, 4 ),
 ( 4.712388980384689674, 6.283185307179586232 ),
 .UNSPECIFIED. ) 
 CURVE ( )  GEOMETRIC_REPRESENTATION_ITEM ( )  RATIONAL_B_SPLINE_CURVE ( ( 1.000000000000000000, 0.8047378541243649375, 0.8047378541243649375, 1.000000000000000000 ) ) 
 REPRESENTATION_ITEM ( '' )  );
#1441 = DIRECTION ( 'NONE',  ( -1.000000000000000000, 0.000000000000000000, -7.663350976776343357E-46 ) ) ;
#1442 = EDGE_CURVE ( 'NONE', #580, #5543, #6223, .T. ) ;
#1443 = DIRECTION ( 'NONE',  ( 0.000000000000000000, 0.000000000000000000, -1.000000000000000000 ) ) ;
#1444 = DIRECTION ( 'NONE',  ( -0.8660254037844410391, 0.000000000000000000, 0.4999999999999959477 ) ) ;
#1445 = CARTESIAN_POINT ( 'NONE',  ( -64.44976119587670382, -223.0636454045093444, 83.68982568666081079 ) ) ;
#1446 = CARTESIAN_POINT ( 'NONE',  ( 187.1032291023277025, -6.494931230503832253, 15.00000000000001066 ) ) ;
#1447 = LINE ( 'NONE', #904, #7007 ) ;
#1448 = EDGE_LOOP ( 'NONE', ( #7159, #6116, #7543, #6796, #5808, #851, #7113, #4585 ) ) ;
#1449 = ORIENTED_EDGE ( 'NONE', *, *, #4917, .T. ) ;
#1450 = PLANE ( 'NONE',  #4761 ) ;
#1451 = CARTESIAN_POINT ( 'NONE',  ( 220.0000000000000000, -56.99999999999999289, 3.000000000000000000 ) ) ;
#1452 = EDGE_CURVE ( 'NONE', #5563, #529, #7331, .T. ) ;
#1453 = CARTESIAN_POINT ( 'NONE',  ( 12.50000000000001066, 12.50000000000001066, -1.214306433183764966E-14 ) ) ;
#1454 = ORIENTED_EDGE ( 'NONE', *, *, #6993, .T. ) ;
#1455 = ORIENTED_EDGE ( 'NONE', *, *, #1775, .T. ) ;
#1456 = CARTESIAN_POINT ( 'NONE',  ( 50.00000000000000000, 0.000000000000000000, 35.00000000000000000 ) ) ;
#1457 = EDGE_CURVE ( 'NONE', #5033, #1231, #2417, .T. ) ;
#1458 = ORIENTED_EDGE ( 'NONE', *, *, #4075, .F. ) ;
#1459 = DIRECTION ( 'NONE',  ( -1.000000000000000000, -0.000000000000000000, -0.000000000000000000 ) ) ;
#1460 = DIRECTION ( 'NONE',  ( 0.000000000000000000, 0.000000000000000000, -1.000000000000000000 ) ) ;
#1461 = ORIENTED_EDGE ( 'NONE', *, *, #6852, .T. ) ;
#1462 = DIRECTION ( 'NONE',  ( 0.000000000000000000, 0.000000000000000000, 1.000000000000000000 ) ) ;
#1463 = CARTESIAN_POINT ( 'NONE',  ( 47.39276988301191551, 27.04312195450870249, 12.73853277175948939 ) ) ;
#1464 = LINE ( 'NONE', #2779, #2883 ) ;
#1465 = VERTEX_POINT ( 'NONE', #1549 ) ;
#1466 = CARTESIAN_POINT ( 'NONE',  ( -60.83909347413332114, -224.0594585235270415, 96.26692417614295039 ) ) ;
#1467 = AXIS2_PLACEMENT_3D ( 'NONE', #4533, #1513, #6832 ) ;
#1468 = DIRECTION ( 'NONE',  ( 0.000000000000000000, 0.000000000000000000, 1.000000000000000000 ) ) ;
#1469 = AXIS2_PLACEMENT_3D ( 'NONE', #676, #4800, #5944 ) ;
#1470 = CARTESIAN_POINT ( 'NONE',  ( 25.00000000000000000, 12.49999999999998401, 9.999999999999996447 ) ) ;
#1471 = EDGE_CURVE ( 'NONE', #6371, #510, #3158, .T. ) ;
#1472 = AXIS2_PLACEMENT_3D ( 'NONE', #2291, #4057, #4557 ) ;
#1473 = CARTESIAN_POINT ( 'NONE',  ( 1.387778780781445676E-14, 73.78679656440351664, 5.999999999999996447 ) ) ;
#1474 = DIRECTION ( 'NONE',  ( 0.000000000000000000, 0.000000000000000000, 1.000000000000000000 ) ) ;
#1475 = DIRECTION ( 'NONE',  ( -1.000000000000000000, -0.000000000000000000, -0.000000000000000000 ) ) ;
#1476 = CARTESIAN_POINT ( 'NONE',  ( -57.52121243805820683, -223.0630252886708149, 74.14711318252129502 ) ) ;
#1477 = CARTESIAN_POINT ( 'NONE',  ( 186.9059892324150098, -5.404540004443668444, 15.00000000000001066 ) ) ;
#1478 = DIRECTION ( 'NONE',  ( 0.000000000000000000, -1.000000000000000000, 0.000000000000000000 ) ) ;
#1479 = AXIS2_PLACEMENT_3D ( 'NONE', #4320, #2004, #5045 ) ;
#1480 = ORIENTED_EDGE ( 'NONE', *, *, #4608, .T. ) ;
#1481 = ORIENTED_EDGE ( 'NONE', *, *, #3523, .F. ) ;
#1482 = AXIS2_PLACEMENT_3D ( 'NONE', #1769, #4126, #3003 ) ;
#1483 = CYLINDRICAL_SURFACE ( 'NONE', #5859, 7.999999999999986677 ) ;
#1484 = CARTESIAN_POINT ( 'NONE',  ( -26.49999999999999289, -99.90626354475344328, 72.90626354475362803 ) ) ;
#1485 = DIRECTION ( 'NONE',  ( 1.000000000000000000, 0.000000000000000000, 0.000000000000000000 ) ) ;
#1486 = ORIENTED_EDGE ( 'NONE', *, *, #4286, .F. ) ;
#1487 = EDGE_CURVE ( 'NONE', #1645, #7378, #6246, .T. ) ;
#1488 = ORIENTED_EDGE ( 'NONE', *, *, #5889, .F. ) ;
#1489 = CIRCLE ( 'NONE', #2723, 6.000000000000019540 ) ;
#1490 = DIRECTION ( 'NONE',  ( 0.000000000000000000, 0.000000000000000000, 1.000000000000000000 ) ) ;
#1491 = EDGE_LOOP ( 'NONE', ( #530, #5499, #1046, #2119, #1309 ) ) ;
#1492 = CARTESIAN_POINT ( 'NONE',  ( -23.84314575050760965, -108.6568542494922127, 36.65685424949233351 ) ) ;
#1493 = FACE_OUTER_BOUND ( 'NONE', #5067, .T. ) ;
#1494 = VERTEX_POINT ( 'NONE', #1473 ) ;
#1495 = EDGE_CURVE ( 'NONE', #4506, #5789, #5565, .T. ) ;
#1496 = CARTESIAN_POINT ( 'NONE',  ( -16.49999999999996447, -49.37258300203045280, 5.999999999999974243 ) ) ;
#1497 = CARTESIAN_POINT ( 'NONE',  ( 48.61993474911651703, 26.84407407967428938, 10.00000000000000888 ) ) ;
#1498 = DIRECTION ( 'NONE',  ( 1.000000000000000000, 1.725633230170963324E-31, -1.078147950931789757E-16 ) ) ;
#1499 = ORIENTED_EDGE ( 'NONE', *, *, #3942, .T. ) ;
#1500 = DIRECTION ( 'NONE',  ( -0.000000000000000000, 0.03489949670250429292, 0.9993908270190955401 ) ) ;
#1501 = DIRECTION ( 'NONE',  ( 0.000000000000000000, -1.000000000000000000, -5.551115123125783935E-17 ) ) ;
#1502 = CARTESIAN_POINT ( 'NONE',  ( -32.50000000000002132, -61.67366827531365914, 34.67366827531376572 ) ) ;
#1503 = B_SPLINE_CURVE_WITH_KNOTS ( 'NONE', 3,
 ( #4814, #3148, #4923, #6727, #3886, #6299, #3304, #1025 ),
 .UNSPECIFIED., .F., .F.,
 ( 4, 2, 2, 4 ),
 ( 0.000000000000000000, 0.4916292630627406846, 0.9738324145908705542, 1.000000000000000000 ),
 .UNSPECIFIED. ) ;
#1504 = VECTOR ( 'NONE', #4058, 1000.000000000000000 ) ;
#1505 = ORIENTED_EDGE ( 'NONE', *, *, #6254, .T. ) ;
#1506 = ORIENTED_EDGE ( 'NONE', *, *, #4001, .T. ) ;
#1507 = CARTESIAN_POINT ( 'NONE',  ( 47.00000000000000000, -21.98659819442010743, 35.76778892745510063 ) ) ;
#1508 = AXIS2_PLACEMENT_3D ( 'NONE', #5142, #6249, #3374 ) ;
#1509 = SURFACE_SIDE_STYLE ('',( #6335 ) ) ;
#1510 = CARTESIAN_POINT ( 'NONE',  ( 25.00000000000000000, 40.21320343559644783, 5.999999999999996447 ) ) ;
#1511 = CARTESIAN_POINT ( 'NONE',  ( 186.0401176793982074, 9.056547830598860926, 13.50026647734630281 ) ) ;
#1512 = CARTESIAN_POINT ( 'NONE',  ( -56.37211203147379734, -223.0620538650801734, 95.72315438295314038 ) ) ;
#1513 = DIRECTION ( 'NONE',  ( 1.000000000000000000, -5.551115123125783935E-17, 4.237045877651919561E-33 ) ) ;
#1514 = FACE_OUTER_BOUND ( 'NONE', #202, .T. ) ;
#1515 = AXIS2_PLACEMENT_3D ( 'NONE', #2286, #5782, #5280 ) ;
#1516 = EDGE_LOOP ( 'NONE', ( #451, #6770, #5098, #2128 ) ) ;
#1517 = ORIENTED_EDGE ( 'NONE', *, *, #6838, .T. ) ;
#1518 = CARTESIAN_POINT ( 'NONE',  ( 13.02230825830123173, -218.0630240738405519, 72.24324488657181575 ) ) ;
#1519 = FACE_BOUND ( 'NONE', #2491, .T. ) ;
#1520 = VECTOR ( 'NONE', #1076, 1000.000000000000000 ) ;
#1521 = EDGE_CURVE ( 'NONE', #3769, #2238, #3780, .T. ) ;
#1522 = LINE ( 'NONE', #2189, #4367 ) ;
#1523 = AXIS2_PLACEMENT_3D ( 'NONE', #7057, #2327, #1789 ) ;
#1524 = AXIS2_PLACEMENT_3D ( 'NONE', #7321, #1614, #6276 ) ;
#1525 = DIRECTION ( 'NONE',  ( 0.000000000000000000, -1.000000000000000000, 0.000000000000000000 ) ) ;
#1526 = ORIENTED_EDGE ( 'NONE', *, *, #1961, .F. ) ;
#1527 = AXIS2_PLACEMENT_3D ( 'NONE', #1230, #3589, #653 ) ;
#1528 = AXIS2_PLACEMENT_3D ( 'NONE', #3603, #3645, #6410 ) ;
#1529 = VERTEX_POINT ( 'NONE', #289 ) ;
#1530 = ADVANCED_FACE ( 'NONE', ( #2635 ), #3834, .T. ) ;
#1531 = CARTESIAN_POINT ( 'NONE',  ( 30.00000000000000000, 0.000000000000000000, 0.000000000000000000 ) ) ;
#1532 = VERTEX_POINT ( 'NONE', #6675 ) ;
#1533 = DIRECTION ( 'NONE',  ( 5.551115123125782702E-17, -0.7071067811865481278, 0.7071067811865469066 ) ) ;
#1534 = AXIS2_PLACEMENT_3D ( 'NONE', #6279, #3321, #1664 ) ;
#1535 = CYLINDRICAL_SURFACE ( 'NONE', #6194, 8.000000000000028422 ) ;
#1536 = ORIENTED_EDGE ( 'NONE', *, *, #5988, .F. ) ;
#1537 = CARTESIAN_POINT ( 'NONE',  ( 47.84883112649161774, 27.19103684831782530, 10.00000000000000711 ) ) ;
#1538 = CARTESIAN_POINT ( 'NONE',  ( -32.50000000000002132, 16.00000000000006750, 32.26953873476009704 ) ) ;
#1539 = EDGE_LOOP ( 'NONE', ( #4296, #1080, #6036, #6386 ) ) ;
#1540 = DIRECTION ( 'NONE',  ( -0.9999999999999997780, 7.351725338072388948E-31, 6.855002664131051427E-29 ) ) ;
#1541 = CARTESIAN_POINT ( 'NONE',  ( -64.50000000000000000, -39.68629150101521219, 24.00000000000002132 ) ) ;
#1542 = EDGE_CURVE ( 'NONE', #6268, #7551, #7360, .T. ) ;
#1543 = DIRECTION ( 'NONE',  ( 7.225445206674839578E-46, -5.551115123125783935E-17, 1.000000000000000000 ) ) ;
#1544 = ADVANCED_FACE ( 'NONE', ( #3294 ), #4446, .T. ) ;
#1545 = FACE_OUTER_BOUND ( 'NONE', #4931, .T. ) ;
#1546 = AXIS2_PLACEMENT_3D ( 'NONE', #2070, #7374, #4419 ) ;
#1547 = EDGE_LOOP ( 'NONE', ( #4430, #3821, #617, #1874, #2822, #3351, #5883, #4240, #544, #1084 ) ) ;
#1548 = ORIENTED_EDGE ( 'NONE', *, *, #5676, .F. ) ;
#1549 = CARTESIAN_POINT ( 'NONE',  ( 50.00000000000000000, 1.714505518806293455E-15, 21.00000000000001066 ) ) ;
#1550 =( NAMED_UNIT ( * ) PLANE_ANGLE_UNIT ( ) SI_UNIT ( $, .RADIAN. ) );
#1551 = CARTESIAN_POINT ( 'NONE',  ( 13.99999999999999645, 0.000000000000000000, -9.999999999999994671 ) ) ;
#1552 = CARTESIAN_POINT ( 'NONE',  ( -59.34588541462897382, -223.0624788587527974, 94.37260828691398729 ) ) ;
#1553 = EDGE_CURVE ( 'NONE', #5460, #4643, #3177, .T. ) ;
#1554 = LINE ( 'NONE', #5639, #6755 ) ;
#1555 = DIRECTION ( 'NONE',  ( 1.000000000000000000, 2.624548829666596385E-30, 9.231085635203014490E-31 ) ) ;
#1556 = CARTESIAN_POINT ( 'NONE',  ( -53.03180245857092956, -218.0630240738404950, 71.94153218116483117 ) ) ;
#1557 = CIRCLE ( 'NONE', #99, 3.000000000000004885 ) ;
#1558 = ORIENTED_EDGE ( 'NONE', *, *, #6596, .T. ) ;
#1559 = ORIENTED_EDGE ( 'NONE', *, *, #5736, .T. ) ;
#1560 = DIRECTION ( 'NONE',  ( 1.000000000000000000, 1.853902270198408060E-44, 1.681558157189780485E-44 ) ) ;
#1561 = DIRECTION ( 'NONE',  ( 1.000000000000000000, 0.000000000000000000, -7.663350976776344912E-46 ) ) ;
#1562 = CARTESIAN_POINT ( 'NONE',  ( 3.000000000000002665, -56.99999999999999289, 7.000000000000000888 ) ) ;
#1563 = FACE_OUTER_BOUND ( 'NONE', #3181, .T. ) ;
#1564 = DIRECTION ( 'NONE',  ( 0.000000000000000000, 0.000000000000000000, -1.000000000000000000 ) ) ;
#1565 = ORIENTED_EDGE ( 'NONE', *, *, #5164, .F. ) ;
#1566 = EDGE_CURVE ( 'NONE', #734, #7349, #5867, .T. ) ;
#1567 = EDGE_LOOP ( 'NONE', ( #5763, #3668 ) ) ;
#1568 = DIRECTION ( 'NONE',  ( 1.311910807449311619E-31, 1.000000000000000000, 0.000000000000000000 ) ) ;
#1569 = ORIENTED_EDGE ( 'NONE', *, *, #5977, .T. ) ;
#1570 = DIRECTION ( 'NONE',  ( -1.000000000000000000, 5.551115123125783935E-17, -4.237045877651919561E-33 ) ) ;
#1571 = CARTESIAN_POINT ( 'NONE',  ( -21.50000000000000355, -114.1489496936987962, 42.14012972382754185 ) ) ;
#1572 = VERTEX_POINT ( 'NONE', #6334 ) ;
#1573 = ADVANCED_FACE ( 'NONE', ( #6285 ), #5212, .F. ) ;
#1574 = CARTESIAN_POINT ( 'NONE',  ( 49.99999999999999289, 24.40605214882040741, 12.96576784911518487 ) ) ;
#1575 = FACE_OUTER_BOUND ( 'NONE', #2891, .T. ) ;
#1576 = EDGE_LOOP ( 'NONE', ( #7215, #2234, #6124, #117 ) ) ;
#1577 = DIRECTION ( 'NONE',  ( 0.5464485389303305185, 1.774256823267135323E-17, -0.8374926831327584864 ) ) ;
#1578 = FACE_OUTER_BOUND ( 'NONE', #6743, .T. ) ;
#1579 = DIRECTION ( 'NONE',  ( -1.000000000000000000, 0.000000000000000000, 0.000000000000000000 ) ) ;
#1580 = CARTESIAN_POINT ( 'NONE',  ( -26.69871789691343267, -115.0146905589846540, 42.92178193144403764 ) ) ;
#1581 = EDGE_LOOP ( 'NONE', ( #4770, #7299, #6612, #7498 ) ) ;
#1582 = ORIENTED_EDGE ( 'NONE', *, *, #4608, .F. ) ;
#1583 = EDGE_CURVE ( 'NONE', #4590, #5645, #3785, .T. ) ;
#1584 = LINE ( 'NONE', #1169, #7216 ) ;
#1585 = CARTESIAN_POINT ( 'NONE',  ( 10.47314606205195631, -223.0630240738404666, 96.09122589815579829 ) ) ;
#1586 = VECTOR ( 'NONE', #5181, 1000.000000000000000 ) ;
#1587 = CARTESIAN_POINT ( 'NONE',  ( 187.4728481691300885, 6.631203003894613701, 15.98182847912006643 ) ) ;
#1588 = CARTESIAN_POINT ( 'NONE',  ( -57.92294587369016767, -223.0630151802142223, 95.13692867617221793 ) ) ;
#1589 = CARTESIAN_POINT ( 'NONE',  ( -12.50000000000001066, -218.0630240738404950, 95.20959099461346398 ) ) ;
#1590 = CARTESIAN_POINT ( 'NONE',  ( 203.9378221735088914, -3.000000000000000888, 38.49999999999998579 ) ) ;
#1591 = CARTESIAN_POINT ( 'NONE',  ( -64.50037575164097348, -218.0629762364925170, 83.76610889236388857 ) ) ;
#1592 = CIRCLE ( 'NONE', #7251, 7.000000000000017764 ) ;
#1593 = ORIENTED_EDGE ( 'NONE', *, *, #7417, .T. ) ;
#1594 = EDGE_CURVE ( 'NONE', #4747, #2183, #6228, .T. ) ;
#1595 = VERTEX_POINT ( 'NONE', #4681 ) ;
#1596 = LINE ( 'NONE', #1635, #2511 ) ;
#1597 = DIRECTION ( 'NONE',  ( 4.930380657631324879E-32, 0.9659258262890683122, -0.2588190451025207950 ) ) ;
#1598 = EDGE_CURVE ( 'NONE', #7269, #105, #4527, .T. ) ;
#1599 = PRODUCT_DEFINITION_SHAPE ( 'NONE', 'NONE',  #7202 ) ;
#1600 = CARTESIAN_POINT ( 'NONE',  ( -26.50000000000003197, -57.68629150101511271, 30.68629150101523351 ) ) ;
#1601 = ADVANCED_BREP_SHAPE_REPRESENTATION ( '', ( #6414, #1914 ), #5969 ) ;
#1602 = CIRCLE ( 'NONE', #5907, 25.00000000000000000 ) ;
#1603 = DIRECTION ( 'NONE',  ( 0.000000000000000000, -1.000000000000000000, -2.065146995210484941E-16 ) ) ;
#1604 = VERTEX_POINT ( 'NONE', #2861 ) ;
#1605 = AXIS2_PLACEMENT_3D ( 'NONE', #2810, #4587, #4085 ) ;
#1606 = ORIENTED_EDGE ( 'NONE', *, *, #1917, .T. ) ;
#1607 = ORIENTED_EDGE ( 'NONE', *, *, #5457, .F. ) ;
#1608 = ADVANCED_FACE ( 'NONE', ( #5756 ), #6408, .F. ) ;
#1609 = LINE ( 'NONE', #6430, #3203 ) ;
#1610 = LINE ( 'NONE', #6314, #5723 ) ;
#1611 = ORIENTED_EDGE ( 'NONE', *, *, #5498, .F. ) ;
#1612 = VECTOR ( 'NONE', #304, 1000.000000000000000 ) ;
#1613 = DIRECTION ( 'NONE',  ( -2.465190328815661892E-32, -1.000000000000000000, -1.193489751472043281E-15 ) ) ;
#1614 = DIRECTION ( 'NONE',  ( 0.000000000000000000, 3.304235192336776498E-16, -1.000000000000000000 ) ) ;
#1615 = ORIENTED_EDGE ( 'NONE', *, *, #6120, .T. ) ;
#1616 = DIRECTION ( 'NONE',  ( 1.000000000000000000, -3.889633291760229481E-29, -3.243011735340676817E-29 ) ) ;
#1617 = EDGE_CURVE ( 'NONE', #4614, #5055, #5431, .T. ) ;
#1618 = CARTESIAN_POINT ( 'NONE',  ( -53.33013951010422460, -219.8343230396700392, 95.52191879319023826 ) ) ;
#1619 = FACE_OUTER_BOUND ( 'NONE', #6981, .T. ) ;
#1620 = CARTESIAN_POINT ( 'NONE',  ( 4.000000000000000000, 0.000000000000000000, 10.00000000000000355 ) ) ;
#1621 = ORIENTED_EDGE ( 'NONE', *, *, #7168, .F. ) ;
#1622 = ORIENTED_EDGE ( 'NONE', *, *, #3151, .F. ) ;
#1623 = DIRECTION ( 'NONE',  ( -1.000000000000000000, 0.000000000000000000, -7.663350976776343357E-46 ) ) ;
#1624 = FILL_AREA_STYLE ('',( #975 ) ) ;
#1625 = EDGE_CURVE ( 'NONE', #4590, #6224, #1090, .T. ) ;
#1626 = CARTESIAN_POINT ( 'NONE',  ( -59.03668131115762918, -223.0625876205039901, 94.56341339751826069 ) ) ;
#1627 = CARTESIAN_POINT ( 'NONE',  ( 21.47795444953126420, -223.0630240738404382, 83.13617250284077898 ) ) ;
#1628 = DIRECTION ( 'NONE',  ( 0.000000000000000000, 0.000000000000000000, -1.000000000000000000 ) ) ;
#1629 = ADVANCED_FACE ( 'NONE', ( #5792 ), #5139, .F. ) ;
#1630 = CARTESIAN_POINT ( 'NONE',  ( -59.02881190857226557, -218.0635488414859537, 73.67786969443412204 ) ) ;
#1631 = VERTEX_POINT ( 'NONE', #511 ) ;
#1632 = CIRCLE ( 'NONE', #7532, 2.999999999999999556 ) ;
#1633 = AXIS2_PLACEMENT_3D ( 'NONE', #7101, #4685, #7022 ) ;
#1634 = VERTEX_POINT ( 'NONE', #3983 ) ;
#1635 = CARTESIAN_POINT ( 'NONE',  ( 220.0000000000000000, 60.00000000000000000, 7.000000000000022204 ) ) ;
#1636 = PLANE ( 'NONE',  #1865 ) ;
#1637 = FACE_BOUND ( 'NONE', #4497, .T. ) ;
#1638 = LINE ( 'NONE', #1067, #5349 ) ;
#1639 = CARTESIAN_POINT ( 'NONE',  ( -13.64230087749234599, -65.63670350735179682, 38.63670350735190340 ) ) ;
#1640 = CIRCLE ( 'NONE', #5580, 15.99999999999999645 ) ;
#1641 = CIRCLE ( 'NONE', #7176, 3.000000000000000000 ) ;
#1642 = EDGE_CURVE ( 'NONE', #6541, #5934, #3416, .T. ) ;
#1643 = EDGE_CURVE ( 'NONE', #6174, #2698, #1584, .T. ) ;
#1644 = PRODUCT_DEFINITION ( 'UNKNOWN', '', #7435, #5946 ) ;
#1645 = VERTEX_POINT ( 'NONE', #476 ) ;
#1646 = ORIENTED_EDGE ( 'NONE', *, *, #3367, .F. ) ;
#1647 = AXIS2_PLACEMENT_3D ( 'NONE', #1726, #5157, #4629 ) ;
#1648 = VECTOR ( 'NONE', #6449, 1000.000000000000000 ) ;
#1649 = AXIS2_PLACEMENT_3D ( 'NONE', #6016, #742, #817 ) ;
#1650 = DIRECTION ( 'NONE',  ( 0.000000000000000000, 0.000000000000000000, 1.000000000000000000 ) ) ;
#1651 = CARTESIAN_POINT ( 'NONE',  ( 217.0000000000000000, 20.99999999999999645, 10.00000000000001066 ) ) ;
#1652 = VERTEX_POINT ( 'NONE', #7443 ) ;
#1653 = CARTESIAN_POINT ( 'NONE',  ( 192.1021416551216419, -6.000000000000000000, 18.00000000000001066 ) ) ;
#1654 = DIRECTION ( 'NONE',  ( 0.000000000000000000, 0.000000000000000000, -1.000000000000000000 ) ) ;
#1655 = AXIS2_PLACEMENT_3D ( 'NONE', #2229, #3923, #3999 ) ;
#1656 = AXIS2_PLACEMENT_3D ( 'NONE', #4902, #2550, #4399 ) ;
#1657 = VECTOR ( 'NONE', #1475, 1000.000000000000000 ) ;
#1658 =( BOUNDED_CURVE ( )  B_SPLINE_CURVE ( 3, ( #7109, #3535, #7562, #2303 ),
 .UNSPECIFIED., .F., .T. ) 
 B_SPLINE_CURVE_WITH_KNOTS ( ( 4, 4 ),
 ( 0.7227342478134169967, 1.570796326794897002 ),
 .UNSPECIFIED. ) 
 CURVE ( )  GEOMETRIC_REPRESENTATION_ITEM ( )  RATIONAL_B_SPLINE_CURVE ( ( 1.000000000000000000, 0.9409585518440986007, 0.9409585518440986007, 1.000000000000000000 ) ) 
 REPRESENTATION_ITEM ( '' )  );
#1659 = EDGE_LOOP ( 'NONE', ( #7277, #7011, #5192, #3270, #880, #2428, #6969, #4161 ) ) ;
#1660 = CARTESIAN_POINT ( 'NONE',  ( 50.03402421525600374, 24.40363903897386422, 9.999999999997291056 ) ) ;
#1661 = CARTESIAN_POINT ( 'NONE',  ( 10.33013951010423170, -219.8343230396699823, 95.52191879319022405 ) ) ;
#1662 =( GEOMETRIC_REPRESENTATION_CONTEXT ( 3 ) GLOBAL_UNCERTAINTY_ASSIGNED_CONTEXT ( ( #3425 ) ) GLOBAL_UNIT_ASSIGNED_CONTEXT ( ( #632, #3486, #5941 ) ) REPRESENTATION_CONTEXT ( 'NONE', 'WORKASPACE' ) );
#1663 = VERTEX_POINT ( 'NONE', #3946 ) ;
#1664 = DIRECTION ( 'NONE',  ( -0.5464485389303294083, -1.427741023604529727E-16, 0.8374926831327591525 ) ) ;
#1665 = LINE ( 'NONE', #4022, #2230 ) ;
#1666 = CARTESIAN_POINT ( 'NONE',  ( 27.99999999999998579, 0.000000000000000000, 0.000000000000000000 ) ) ;
#1667 = APPLICATION_CONTEXT ( 'automotive_design' ) ;
#1668 = ORIENTED_EDGE ( 'NONE', *, *, #1947, .F. ) ;
#1669 = VERTEX_POINT ( 'NONE', #7554 ) ;
#1670 = EDGE_CURVE ( 'NONE', #105, #7581, #1013, .T. ) ;
#1671 = DIRECTION ( 'NONE',  ( 0.000000000000000000, 0.000000000000000000, -1.000000000000000000 ) ) ;
#1672 = DIRECTION ( 'NONE',  ( 0.000000000000000000, 0.000000000000000000, -1.000000000000000000 ) ) ;
#1673 = CARTESIAN_POINT ( 'NONE',  ( 217.0000000000000000, 60.00000000000000000, 7.000000000000022204 ) ) ;
#1674 = DIRECTION ( 'NONE',  ( 1.000000000000000000, 2.465190328815661892E-32, -9.244463733058732095E-33 ) ) ;
#1675 = DIRECTION ( 'NONE',  ( -1.000000000000000000, -1.725633230170963324E-31, 1.078147950931789387E-16 ) ) ;
#1676 = CARTESIAN_POINT ( 'NONE',  ( 25.00000000000002132, 0.000000000000000000, -1.734723475976807094E-15 ) ) ;
#1677 = CARTESIAN_POINT ( 'NONE',  ( -54.49733181648158364, -218.0639264276503297, 72.01289010251366562 ) ) ;
#1678 = ORIENTED_EDGE ( 'NONE', *, *, #5058, .F. ) ;
#1679 = VECTOR ( 'NONE', #3775, 1000.000000000000000 ) ;
#1680 = ADVANCED_FACE ( 'NONE', ( #6982 ), #442, .F. ) ;
#1681 = ORIENTED_EDGE ( 'NONE', *, *, #1594, .T. ) ;
#1682 = CARTESIAN_POINT ( 'NONE',  ( 11.55538789554288037, -218.0630240738405519, 71.94153218116487380 ) ) ;
#1683 = DIRECTION ( 'NONE',  ( 1.000000000000000000, 0.000000000000000000, 0.000000000000000000 ) ) ;
#1684 = LINE ( 'NONE', #6959, #4114 ) ;
#1685 = CARTESIAN_POINT ( 'NONE',  ( 220.0000000000000000, 56.99999999999999289, 7.000000000000022204 ) ) ;
#1686 = CARTESIAN_POINT ( 'NONE',  ( 188.7282013335461670, -8.214756345321047704, 15.07808197065826405 ) ) ;
#1687 = AXIS2_PLACEMENT_3D ( 'NONE', #2806, #3753, #243 ) ;
#1688 = ORIENTED_EDGE ( 'NONE', *, *, #219, .T. ) ;
#1689 = ORIENTED_EDGE ( 'NONE', *, *, #3447, .T. ) ;
#1690 = EDGE_CURVE ( 'NONE', #3560, #7581, #179, .T. ) ;
#1691 = DIRECTION ( 'NONE',  ( -1.000000000000000000, 5.551115123125783935E-17, -4.237045877651919561E-33 ) ) ;
#1692 = CARTESIAN_POINT ( 'NONE',  ( 220.0000000000000000, -9.000000000000001776, 18.00000000000001066 ) ) ;
#1693 = ORIENTED_EDGE ( 'NONE', *, *, #2515, .F. ) ;
#1694 = DIRECTION ( 'NONE',  ( -1.000000000000000000, -2.465190328815661892E-32, 9.244463733058732095E-33 ) ) ;
#1695 = LINE ( 'NONE', #3626, #5593 ) ;
#1696 = ORIENTED_EDGE ( 'NONE', *, *, #3608, .T. ) ;
#1697 = ORIENTED_EDGE ( 'NONE', *, *, #196, .T. ) ;
#1698 = ADVANCED_FACE ( 'NONE', ( #3482 ), #399, .F. ) ;
#1699 = CARTESIAN_POINT ( 'NONE',  ( 10.25759302228802738, -223.0630240738404382, 73.28127814332047762 ) ) ;
#1700 = DIRECTION ( 'NONE',  ( -0.000000000000000000, 0.000000000000000000, 1.000000000000000000 ) ) ;
#1701 = EDGE_LOOP ( 'NONE', ( #4907, #4460, #2033, #5024 ) ) ;
#1702 = APPLICATION_PROTOCOL_DEFINITION ( 'draft international standard', 'automotive_design', 1998, #4036 ) ;
#1703 = CARTESIAN_POINT ( 'NONE',  ( 25.00000000000002132, 82.46446609406720540, 6.464466094067254254 ) ) ;
#1704 = LINE ( 'NONE', #4096, #169 ) ;
#1705 = ORIENTED_EDGE ( 'NONE', *, *, #3108, .T. ) ;
#1706 = ORIENTED_EDGE ( 'NONE', *, *, #3822, .T. ) ;
#1707 = CARTESIAN_POINT ( 'NONE',  ( 2.775557561562891351E-14, 28.00000000000002487, 9.999999999999992895 ) ) ;
#1708 =( LENGTH_UNIT ( ) NAMED_UNIT ( * ) SI_UNIT ( .MILLI., .METRE. ) );
#1709 = DIRECTION ( 'NONE',  ( 1.000000000000000000, 0.000000000000000000, 0.000000000000000000 ) ) ;
#1710 = CARTESIAN_POINT ( 'NONE',  ( 3.000000000000002665, -60.00000000000000000, 10.00000000000000000 ) ) ;
#1711 = LINE ( 'NONE', #7063, #4189 ) ;
#1712 = ADVANCED_FACE ( 'NONE', ( #4721 ), #1281, .T. ) ;
#1713 = ORIENTED_EDGE ( 'NONE', *, *, #7061, .T. ) ;
#1714 = AXIS2_PLACEMENT_3D ( 'NONE', #1666, #4558, #2784 ) ;
#1715 = LINE ( 'NONE', #6676, #5465 ) ;
#1716 = DIRECTION ( 'NONE',  ( 0.000000000000000000, 1.836970198721029934E-16, -1.000000000000000000 ) ) ;
#1717 = LINE ( 'NONE', #486, #4363 ) ;
#1718 = CARTESIAN_POINT ( 'NONE',  ( 200.0000000000000000, 0.000000000000000000, 0.000000000000000000 ) ) ;
#1719 = DIRECTION ( 'NONE',  ( -1.000000000000000000, 1.294224922628222493E-31, -1.078147950931789264E-16 ) ) ;
#1720 = CIRCLE ( 'NONE', #4426, 7.999999999999986677 ) ;
#1721 = AXIS2_PLACEMENT_3D ( 'NONE', #6754, #295, #6066 ) ;
#1722 = ORIENTED_EDGE ( 'NONE', *, *, #307, .T. ) ;
#1723 = ORIENTED_EDGE ( 'NONE', *, *, #7327, .T. ) ;
#1724 = VECTOR ( 'NONE', #6324, 1000.000000000000000 ) ;
#1725 = FACE_OUTER_BOUND ( 'NONE', #5005, .T. ) ;
#1726 = CARTESIAN_POINT ( 'NONE',  ( 170.0000000000000000, 0.000000000000000000, 0.000000000000000000 ) ) ;
#1727 = ORIENTED_EDGE ( 'NONE', *, *, #993, .T. ) ;
#1728 = ADVANCED_FACE ( 'NONE', ( #6521 ), #6014, .F. ) ;
#1729 = CARTESIAN_POINT ( 'NONE',  ( -29.35769912250765046, -65.63670350735181103, 38.63670350735190340 ) ) ;
#1730 = PLANE ( 'NONE',  #4493 ) ;
#1731 = VECTOR ( 'NONE', #6187, 1000.000000000000000 ) ;
#1732 = ADVANCED_FACE ( 'NONE', ( #4179 ), #1939, .F. ) ;
#1733 = ORIENTED_EDGE ( 'NONE', *, *, #3849, .T. ) ;
#1734 = ORIENTED_EDGE ( 'NONE', *, *, #4763, .F. ) ;
#1735 = CARTESIAN_POINT ( 'NONE',  ( -21.50000000000000000, -215.0630240738403813, -2.775557561562891351E-13 ) ) ;
#1736 = CARTESIAN_POINT ( 'NONE',  ( 10.00237955168283044, -212.4343899438498511, 94.21711093295958506 ) ) ;
#1737 = EDGE_LOOP ( 'NONE', ( #6956, #7125, #7575, #562 ) ) ;
#1738 = ITEM_DEFINED_TRANSFORMATION ( 'NONE', 'NONE', #201,  #1914 ) ;
#1739 = DIRECTION ( 'NONE',  ( 0.4999999999999976130, 0.000000000000000000, 0.8660254037844399289 ) ) ;
#1740 = CARTESIAN_POINT ( 'NONE',  ( 217.0000000000000000, 56.99999999999999289, 7.000000000000022204 ) ) ;
#1741 = EDGE_CURVE ( 'NONE', #3993, #4453, #2309, .T. ) ;
#1742 = PRODUCT_DEFINITION_SHAPE ( 'NONE', 'NONE',  #3590 ) ;
#1743 = ORIENTED_EDGE ( 'NONE', *, *, #1643, .F. ) ;
#1744 = PRODUCT_DEFINITION ( 'UNKNOWN', '', #2154, #3229 ) ;
#1745 = DIRECTION ( 'NONE',  ( 1.000000000000000000, -5.551115123125783935E-17, 4.237045877651919561E-33 ) ) ;
#1746 = AXIS2_PLACEMENT_3D ( 'NONE', #3171, #1974, #6669 ) ;
#1747 = DIRECTION ( 'NONE',  ( -0.000000000000000000, 0.000000000000000000, 1.000000000000000000 ) ) ;
#1748 =( BOUNDED_CURVE ( )  B_SPLINE_CURVE ( 3, ( #4665, #4546, #2724, #6997 ),
 .UNSPECIFIED., .F., .T. ) 
 B_SPLINE_CURVE_WITH_KNOTS ( ( 4, 4 ),
 ( 0.000000000000000000, 3.141592653589793116 ),
 .UNSPECIFIED. ) 
 CURVE ( )  GEOMETRIC_REPRESENTATION_ITEM ( )  RATIONAL_B_SPLINE_CURVE ( ( 1.000000000000000000, 0.3333333333333333703, 0.3333333333333333703, 1.000000000000000000 ) ) 
 REPRESENTATION_ITEM ( '' )  );
#1749 = CARTESIAN_POINT ( 'NONE',  ( 0.000000000000000000, 0.000000000000000000, 0.000000000000000000 ) ) ;
#1750 = CYLINDRICAL_SURFACE ( 'NONE', #173, 6.000000000000001776 ) ;
#1751 = CARTESIAN_POINT ( 'NONE',  ( 20.79427630190120269, -223.0630240738404950, 88.78961924518958426 ) ) ;
#1752 = CARTESIAN_POINT ( 'NONE',  ( 192.1021416551216419, 6.000000000000000000, 18.00000000000001066 ) ) ;
#1753 = VERTEX_POINT ( 'NONE', #3642 ) ;
#1754 = VERTEX_POINT ( 'NONE', #6597 ) ;
#1755 = DIRECTION ( 'NONE',  ( 1.000000000000000000, 0.000000000000000000, 7.663350976776343357E-46 ) ) ;
#1756 = DIRECTION ( 'NONE',  ( 1.000000000000000000, 0.000000000000000000, -5.605193857299270773E-45 ) ) ;
#1757 = CARTESIAN_POINT ( 'NONE',  ( 2.775557561562891351E-14, 86.00000000000000000, 9.999999999999996447 ) ) ;
#1758 = FACE_BOUND ( 'NONE', #5123, .T. ) ;
#1759 = ORIENTED_EDGE ( 'NONE', *, *, #7005, .F. ) ;
#1760 = ORIENTED_EDGE ( 'NONE', *, *, #6853, .F. ) ;
#1761 = ADVANCED_FACE ( 'NONE', ( #1824, #1896 ), #5938, .F. ) ;
#1762 = DIRECTION ( 'NONE',  ( 0.000000000000000000, 0.000000000000000000, 1.000000000000000000 ) ) ;
#1763 = ADVANCED_FACE ( 'NONE', ( #5324, #2516 ), #741, .F. ) ;
#1764 = AXIS2_PLACEMENT_3D ( 'NONE', #6046, #5972, #7199 ) ;
#1765 = CYLINDRICAL_SURFACE ( 'NONE', #1772, 2.999999999999999112 ) ;
#1766 = AXIS2_PLACEMENT_3D ( 'NONE', #6337, #3949, #6290 ) ;
#1767 = ORIENTED_EDGE ( 'NONE', *, *, #7237, .F. ) ;
#1768 = CARTESIAN_POINT ( 'NONE',  ( -52.98766809822285495, -217.0856944719845671, 71.67965750360849597 ) ) ;
#1769 = CARTESIAN_POINT ( 'NONE',  ( 0.000000000000000000, 0.000000000000000000, -6.999999999999992006 ) ) ;
#1770 = CYLINDRICAL_SURFACE ( 'NONE', #1291, 2.999999999999999112 ) ;
#1771 = EDGE_LOOP ( 'NONE', ( #1884, #2354 ) ) ;
#1772 = AXIS2_PLACEMENT_3D ( 'NONE', #4123, #6505, #6467 ) ;
#1773 = AXIS2_PLACEMENT_3D ( 'NONE', #5983, #6629, #3169 ) ;
#1774 = ORIENTED_EDGE ( 'NONE', *, *, #5786, .F. ) ;
#1775 = EDGE_CURVE ( 'NONE', #429, #233, #2403, .T. ) ;
#1776 = DIRECTION ( 'NONE',  ( 5.551115123125783935E-17, 1.000000000000000000, -2.214819436045321778E-32 ) ) ;
#1777 = CARTESIAN_POINT ( 'NONE',  ( 217.0000000000000000, -56.99999999999999289, 10.00000000000000000 ) ) ;
#1778 = ORIENTED_EDGE ( 'NONE', *, *, #2042, .F. ) ;
#1779 = CONTEXT_DEPENDENT_SHAPE_REPRESENTATION ( #2162, #7114 ) ;
#1780 = AXIS2_PLACEMENT_3D ( 'NONE', #7555, #5903, #6983 ) ;
#1781 = CYLINDRICAL_SURFACE ( 'NONE', #5295, 5.000000000000009770 ) ;
#1782 = CIRCLE ( 'NONE', #2399, 7.999999999999986677 ) ;
#1783 = DIRECTION ( 'NONE',  ( -0.000000000000000000, 0.000000000000000000, 1.000000000000000000 ) ) ;
#1784 = ORIENTED_EDGE ( 'NONE', *, *, #3041, .F. ) ;
#1785 = CIRCLE ( 'NONE', #4751, 9.999999999999998224 ) ;
#1786 = AXIS2_PLACEMENT_3D ( 'NONE', #4021, #889, #3246 ) ;
#1787 = CARTESIAN_POINT ( 'NONE',  ( 25.00000000000001421, 35.07106781186547551, 2.928932188134525827 ) ) ;
#1788 = EDGE_CURVE ( 'NONE', #722, #2384, #3677, .T. ) ;
#1789 = DIRECTION ( 'NONE',  ( 1.000000000000000000, 0.000000000000000000, -5.605193857299270773E-45 ) ) ;
#1790 = CARTESIAN_POINT ( 'NONE',  ( 21.50000000000000000, -99.90626354475340065, 72.90626354475362803 ) ) ;
#1791 = CARTESIAN_POINT ( 'NONE',  ( 10.25168462842736261, -218.0630240738404950, 95.20959099461346398 ) ) ;
#1792 = CARTESIAN_POINT ( 'NONE',  ( 16.21315755988861440, -223.0630240738403813, 74.98638948672413562 ) ) ;
#1793 = CARTESIAN_POINT ( 'NONE',  ( -20.67719663180526624, -65.17719663180515965, 38.17719663180528045 ) ) ;
#1794 = PRODUCT_DEFINITION_CONTEXT ( 'detailed design', #1667, 'design' ) ;
#1795 = ORIENTED_EDGE ( 'NONE', *, *, #3731, .T. ) ;
#1796 = VERTEX_POINT ( 'NONE', #102 ) ;
#1797 = DIRECTION ( 'NONE',  ( 1.000000000000000000, 0.000000000000000000, 0.000000000000000000 ) ) ;
#1798 = ADVANCED_FACE ( 'NONE', ( #3024 ), #7099, .T. ) ;
#1799 = DIRECTION ( 'NONE',  ( -1.000000000000000000, 0.000000000000000000, 0.000000000000000000 ) ) ;
#1800 = FACE_BOUND ( 'NONE', #225, .T. ) ;
#1801 = DIRECTION ( 'NONE',  ( -0.4999999999999976130, -0.000000000000000000, -0.8660254037844399289 ) ) ;
#1802 = DIRECTION ( 'NONE',  ( 7.623657272262514668E-17, -0.7071067811865465735, 0.7071067811865485719 ) ) ;
#1803 = DIRECTION ( 'NONE',  ( 0.000000000000000000, -1.000000000000000000, -1.221245327087672392E-15 ) ) ;
#1804 = VECTOR ( 'NONE', #1597, 1000.000000000000114 ) ;
#1805 = ORIENTED_EDGE ( 'NONE', *, *, #941, .F. ) ;
#1806 = ORIENTED_EDGE ( 'NONE', *, *, #2983, .T. ) ;
#1807 = CARTESIAN_POINT ( 'NONE',  ( 25.00000000000000711, 40.21320343559642652, 10.99999999999999467 ) ) ;
#1808 = VECTOR ( 'NONE', #4152, 1000.000000000000000 ) ;
#1809 = DIRECTION ( 'NONE',  ( 1.000000000000000000, -5.551115123125783935E-17, 4.237045877651919561E-33 ) ) ;
#1810 = ORIENTED_EDGE ( 'NONE', *, *, #5263, .T. ) ;
#1811 = CARTESIAN_POINT ( 'NONE',  ( -70.14230383934500423, -220.9072961629242968, 78.53943569403833180 ) ) ;
#1812 = FACE_OUTER_BOUND ( 'NONE', #407, .T. ) ;
#1813 = CARTESIAN_POINT ( 'NONE',  ( 50.00000000000000000, 0.000000000000000000, 35.00000000000000000 ) ) ;
#1814 = EDGE_CURVE ( 'NONE', #2614, #2574, #7462, .T. ) ;
#1815 = EDGE_LOOP ( 'NONE', ( #1089, #7121, #4206, #1412, #4899, #6208, #3157 ) ) ;
#1816 = AXIS2_PLACEMENT_3D ( 'NONE', #590, #1244, #1861 ) ;
#1817 = ORIENTED_EDGE ( 'NONE', *, *, #2873, .F. ) ;
#1818 = CYLINDRICAL_SURFACE ( 'NONE', #665, 17.99999999999999645 ) ;
#1819 = CARTESIAN_POINT ( 'NONE',  ( 3.000000000000000000, -56.99999999999999289, 7.000000000000000888 ) ) ;
#1820 = ORIENTED_EDGE ( 'NONE', *, *, #80, .F. ) ;
#1821 = CARTESIAN_POINT ( 'NONE',  ( 217.0000000000000000, -9.000000000000001776, 15.00000000000000888 ) ) ;
#1822 = FACE_OUTER_BOUND ( 'NONE', #2715, .T. ) ;
#1823 = EDGE_LOOP ( 'NONE', ( #1349, #2669, #262, #1678 ) ) ;
#1824 = FACE_BOUND ( 'NONE', #5461, .T. ) ;
#1825 = CARTESIAN_POINT ( 'NONE',  ( -32.50000000000002842, -49.37258300203047412, 0.000000000000000000 ) ) ;
#1826 = DIRECTION ( 'NONE',  ( 5.551115123125783935E-17, 1.000000000000000000, -2.214819436045321778E-32 ) ) ;
#1827 = LINE ( 'NONE', #216, #1842 ) ;
#1828 = CARTESIAN_POINT ( 'NONE',  ( 3.000000000000002665, 60.00000000000000000, 7.000000000000023093 ) ) ;
#1829 = ADVANCED_FACE ( 'NONE', ( #4217, #170 ), #5405, .F. ) ;
#1830 = B_SPLINE_CURVE_WITH_KNOTS ( 'NONE', 3,
 ( #922, #2078, #5620, #343 ),
 .UNSPECIFIED., .F., .F.,
 ( 4, 4 ),
 ( 1.734723475976807094E-18, 0.0005182278649586899693 ),
 .UNSPECIFIED. ) ;
#1831 = DIRECTION ( 'NONE',  ( 4.930380657631323236E-32, 0.9848077530122080203, -0.1736481776669304422 ) ) ;
#1832 = CARTESIAN_POINT ( 'NONE',  ( 220.0000000000000000, 20.99999999999999645, 7.000000000000009770 ) ) ;
#1833 = CARTESIAN_POINT ( 'NONE',  ( -26.50000000000003197, -49.37258300203047412, 6.000000000000002665 ) ) ;
#1834 = CARTESIAN_POINT ( 'NONE',  ( 186.9059892324150951, 5.404544942268280749, 15.00000000000001421 ) ) ;
#1835 = CARTESIAN_POINT ( 'NONE',  ( 200.0000000000000000, 1.714505518806294244E-15, -13.99999999999999822 ) ) ;
#1836 = EDGE_CURVE ( 'NONE', #2926, #908, #4288, .T. ) ;
#1837 = ORIENTED_EDGE ( 'NONE', *, *, #2696, .T. ) ;
#1838 = EDGE_LOOP ( 'NONE', ( #7165, #4210, #1368, #153 ) ) ;
#1839 = EDGE_CURVE ( 'NONE', #647, #1652, #1557, .T. ) ;
#1840 = CARTESIAN_POINT ( 'NONE',  ( -15.92209785380265608, -113.7796841263388501, 41.77968412633906325 ) ) ;
#1841 = CARTESIAN_POINT ( 'NONE',  ( -64.50000000000000000, 0.000000000000000000, 0.000000000000000000 ) ) ;
#1842 = VECTOR ( 'NONE', #1867, 1000.000000000000000 ) ;
#1843 = VERTEX_POINT ( 'NONE', #4140 ) ;
#1844 = AXIS2_PLACEMENT_3D ( 'NONE', #7024, #7138, #1868 ) ;
#1845 = CARTESIAN_POINT ( 'NONE',  ( -70.08493024494319457, -221.0431231857560306, 90.06937369499782164 ) ) ;
#1846 = SURFACE_STYLE_USAGE ( .BOTH. , #4784 ) ;
#1847 = CARTESIAN_POINT ( 'NONE',  ( -63.69261809097343274, -218.0630232800231738, 87.98794966951278695 ) ) ;
#1848 = ORIENTED_EDGE ( 'NONE', *, *, #5539, .T. ) ;
#1849 = VECTOR ( 'NONE', #4522, 1000.000000000000000 ) ;
#1850 = ORIENTED_EDGE ( 'NONE', *, *, #4624, .F. ) ;
#1851 = EDGE_CURVE ( 'NONE', #2809, #4322, #6485, .T. ) ;
#1852 = LINE ( 'NONE', #4208, #2877 ) ;
#1853 = CARTESIAN_POINT ( 'NONE',  ( 17.76462208873361348, -223.8662738488898185, 73.49650827185845969 ) ) ;
#1854 = ORIENTED_EDGE ( 'NONE', *, *, #4508, .T. ) ;
#1855 = APPLICATION_PROTOCOL_DEFINITION ( 'draft international standard', 'automotive_design', 1998, #4822 ) ;
#1856 = CIRCLE ( 'NONE', #3591, 17.99999999999999645 ) ;
#1857 = DIRECTION ( 'NONE',  ( 1.000000000000000000, 2.624548829666596736E-30, -9.231085635203017994E-31 ) ) ;
#1858 = DIRECTION ( 'NONE',  ( -2.465190328815662439E-32, -0.7071067811865464625, 0.7071067811865485719 ) ) ;
#1859 = ORIENTED_EDGE ( 'NONE', *, *, #124, .F. ) ;
#1860 = CIRCLE ( 'NONE', #1482, 26.99999999999999289 ) ;
#1861 = DIRECTION ( 'NONE',  ( -1.751623080406021728E-46, 0.9848077530122081313, -0.1736481776669305255 ) ) ;
#1862 = ADVANCED_FACE ( 'NONE', ( #927, #3283, #6092, #5738, #460 ), #816, .F. ) ;
#1863 = DIRECTION ( 'NONE',  ( 3.081487911019577365E-33, 1.193489751472043281E-15, -1.000000000000000000 ) ) ;
#1864 = DIRECTION ( 'NONE',  ( 1.000000000000000000, 0.000000000000000000, 0.000000000000000000 ) ) ;
#1865 = AXIS2_PLACEMENT_3D ( 'NONE', #1216, #3996, #3572 ) ;
#1866 = CARTESIAN_POINT ( 'NONE',  ( 13.22237817618507805, -218.0630240738405234, 94.81205485192671745 ) ) ;
#1867 = DIRECTION ( 'NONE',  ( -1.000000000000000000, -2.624548829666596736E-30, 9.231085635203017994E-31 ) ) ;
#1868 = DIRECTION ( 'NONE',  ( 0.000000000000000000, 0.000000000000000000, 1.000000000000000000 ) ) ;
#1869 = DIRECTION ( 'NONE',  ( -1.000000000000000000, 0.000000000000000000, -7.663350976776343357E-46 ) ) ;
#1870 = EDGE_CURVE ( 'NONE', #580, #5858, #5156, .T. ) ;
#1871 = PRESENTATION_STYLE_ASSIGNMENT (( #3571 ) ) ;
#1872 = CYLINDRICAL_SURFACE ( 'NONE', #2361, 3.000000000000001332 ) ;
#1873 = CARTESIAN_POINT ( 'NONE',  ( 188.3801170496620045, 8.732029405377334186, 15.00000000000001066 ) ) ;
#1874 = ORIENTED_EDGE ( 'NONE', *, *, #3382, .T. ) ;
#1875 = ORIENTED_EDGE ( 'NONE', *, *, #4005, .T. ) ;
#1876 = CARTESIAN_POINT ( 'NONE',  ( -16.49999999999996803, 16.00000000000006395, 30.68629150101531877 ) ) ;
#1877 = DIRECTION ( 'NONE',  ( 0.000000000000000000, 0.000000000000000000, 1.000000000000000000 ) ) ;
#1878 = EDGE_CURVE ( 'NONE', #1465, #3492, #4435, .T. ) ;
#1879 = ADVANCED_FACE ( 'NONE', ( #5018 ), #2009, .T. ) ;
#1880 = CARTESIAN_POINT ( 'NONE',  ( -70.16044999292957129, -217.6494054747795417, 89.39435792273813775 ) ) ;
#1881 = AXIS2_PLACEMENT_3D ( 'NONE', #98, #2360, #3522 ) ;
#1882 = CARTESIAN_POINT ( 'NONE',  ( -26.50000000000002842, -49.37258300203047412, -16.00000000000004263 ) ) ;
#1883 = DIRECTION ( 'NONE',  ( 1.000000000000000000, 0.000000000000000000, 0.000000000000000000 ) ) ;
#1884 = ORIENTED_EDGE ( 'NONE', *, *, #2621, .T. ) ;
#1885 = ORIENTED_EDGE ( 'NONE', *, *, #2468, .T. ) ;
#1886 = AXIS2_PLACEMENT_3D ( 'NONE', #1093, #1017, #4490 ) ;
#1887 = DIRECTION ( 'NONE',  ( 1.000000000000000000, 0.000000000000000000, 0.000000000000000000 ) ) ;
#1888 = CARTESIAN_POINT ( 'NONE',  ( 27.14230383934499002, -220.9072961629242116, 78.53943569403831759 ) ) ;
#1889 = ADVANCED_FACE ( 'NONE', ( #5518 ), #3202, .F. ) ;
#1890 = ORIENTED_EDGE ( 'NONE', *, *, #6093, .T. ) ;
#1891 = CARTESIAN_POINT ( 'NONE',  ( 217.0000000000000000, -9.000000000000001776, 12.00000000000000711 ) ) ;
#1892 = CARTESIAN_POINT ( 'NONE',  ( 220.0000000000000000, 0.000000000000000000, 0.000000000000000000 ) ) ;
#1893 = CIRCLE ( 'NONE', #4977, 15.99999999999999645 ) ;
#1894 = TOROIDAL_SURFACE ( 'NONE', #2878, 6.000000000000000000, 3.000000000000000000 ) ;
#1895 = VERTEX_POINT ( 'NONE', #6777 ) ;
#1896 = FACE_OUTER_BOUND ( 'NONE', #1567, .T. ) ;
#1897 = AXIS2_PLACEMENT_3D ( 'NONE', #1841, #4199, #6544 ) ;
#1898 = AXIS2_PLACEMENT_3D ( 'NONE', #1825, #6373, #592 ) ;
#1899 = DIRECTION ( 'NONE',  ( -4.622231866529368100E-33, 2.600005424922769496E-32, -1.000000000000000000 ) ) ;
#1900 = AXIS2_PLACEMENT_3D ( 'NONE', #3195, #2228, #6258 ) ;
#1901 = SHAPE_REPRESENTATION_RELATIONSHIP ( 'NONE' , 'NONE' ,  #867, #7208 ) ;
#1902 = DIRECTION ( 'NONE',  ( -6.162975822039153361E-33, -5.166928274020107963E-17, 1.000000000000000000 ) ) ;
#1903 = DIRECTION ( 'NONE',  ( 1.000000000000000000, 0.000000000000000000, 0.000000000000000000 ) ) ;
#1904 = DIRECTION ( 'NONE',  ( 1.000000000000000000, 0.000000000000000000, 5.605193857299269528E-45 ) ) ;
#1905 = EDGE_CURVE ( 'NONE', #5154, #6636, #7350, .T. ) ;
#1906 = AXIS2_PLACEMENT_3D ( 'NONE', #3315, #6152, #882 ) ;
#1907 = AXIS2_PLACEMENT_3D ( 'NONE', #900, #3763, #3143 ) ;
#1908 = EDGE_CURVE ( 'NONE', #5322, #5661, #4366, .T. ) ;
#1909 = ORIENTED_EDGE ( 'NONE', *, *, #5767, .F. ) ;
#1910 = LINE ( 'NONE', #1326, #3038 ) ;
#1911 = CARTESIAN_POINT ( 'NONE',  ( 2.000000000000001776, 0.000000000000000000, 0.000000000000000000 ) ) ;
#1912 = DIRECTION ( 'NONE',  ( -1.000000000000000000, 5.551115123125783935E-17, -4.237045877651919561E-33 ) ) ;
#1913 = CARTESIAN_POINT ( 'NONE',  ( -63.46819182528941639, -223.0630670020534296, 79.98999288546480102 ) ) ;
#1914 = AXIS2_PLACEMENT_3D ( 'NONE', #1749, #62, #1864 ) ;
#1915 = CARTESIAN_POINT ( 'NONE',  ( 187.9926472795798702, -6.022797726957934472, 16.88214694814191219 ) ) ;
#1916 = APPLICATION_CONTEXT ( 'automotive_design' ) ;
#1917 = EDGE_CURVE ( 'NONE', #7550, #6856, #4583, .T. ) ;
#1918 = ORIENTED_EDGE ( 'NONE', *, *, #772, .F. ) ;
#1919 = VERTEX_POINT ( 'NONE', #3712 ) ;
#1920 = FACE_OUTER_BOUND ( 'NONE', #415, .T. ) ;
#1921 = CYLINDRICAL_SURFACE ( 'NONE', #4484, 15.99999999999998934 ) ;
#1922 = CARTESIAN_POINT ( 'NONE',  ( -70.00607124224620748, -226.9703646923684914, 80.02312588464759813 ) ) ;
#1923 = CIRCLE ( 'NONE', #693, 26.99999999999999289 ) ;
#1924 = DIRECTION ( 'NONE',  ( -1.000000000000000000, -0.000000000000000000, -7.663350976776343357E-46 ) ) ;
#1925 = CARTESIAN_POINT ( 'NONE',  ( -64.32060244815615135, -218.0610728454553850, 85.77987718927815308 ) ) ;
#1926 = VERTEX_POINT ( 'NONE', #1496 ) ;
#1927 = EDGE_CURVE ( 'NONE', #238, #6147, #3860, .T. ) ;
#1928 = ORIENTED_EDGE ( 'NONE', *, *, #5003, .F. ) ;
#1929 = AXIS2_PLACEMENT_3D ( 'NONE', #1253, #70, #1831 ) ;
#1930 = CARTESIAN_POINT ( 'NONE',  ( 21.50000000000000000, -99.90626354475340065, 72.90626354475362803 ) ) ;
#1931 = CARTESIAN_POINT ( 'NONE',  ( 27.24145449743711112, -216.4945693450225974, 77.45959972289220730 ) ) ;
#1932 = VERTEX_POINT ( 'NONE', #1350 ) ;
#1933 = DIRECTION ( 'NONE',  ( 0.000000000000000000, 0.000000000000000000, -1.000000000000000000 ) ) ;
#1934 = CARTESIAN_POINT ( 'NONE',  ( 6.500000000000000888, 101.5000000000000000, 4.999999999999999112 ) ) ;
#1935 = VECTOR ( 'NONE', #4062, 1000.000000000000114 ) ;
#1936 = VERTEX_POINT ( 'NONE', #775 ) ;
#1937 = EDGE_CURVE ( 'NONE', #3401, #1241, #7456, .T. ) ;
#1938 = EDGE_CURVE ( 'NONE', #959, #4660, #7098, .T. ) ;
#1939 = CYLINDRICAL_SURFACE ( 'NONE', #3287, 7.999999999999986677 ) ;
#1940 = VERTEX_POINT ( 'NONE', #4905 ) ;
#1941 = CARTESIAN_POINT ( 'NONE',  ( 21.50000000000000000, -39.68629150101521219, 16.00000000000001421 ) ) ;
#1942 = DIRECTION ( 'NONE',  ( -1.000000000000000000, 0.000000000000000000, 0.000000000000000000 ) ) ;
#1943 = ORIENTED_EDGE ( 'NONE', *, *, #6546, .T. ) ;
#1944 = CARTESIAN_POINT ( 'NONE',  ( 21.50000000000000000, -60.68629150101523351, -11.31370849898472031 ) ) ;
#1945 =( NAMED_UNIT ( * ) PLANE_ANGLE_UNIT ( ) SI_UNIT ( $, .RADIAN. ) );
#1946 = DIRECTION ( 'NONE',  ( -1.000000000000000000, 0.000000000000000000, 0.000000000000000000 ) ) ;
#1947 = EDGE_CURVE ( 'NONE', #3211, #5002, #4646, .T. ) ;
#1948 = CARTESIAN_POINT ( 'NONE',  ( -63.76541543211998686, -223.0629989142765339, 88.86326335188097403 ) ) ;
#1949 = EDGE_CURVE ( 'NONE', #3811, #2040, #2620, .T. ) ;
#1950 = CARTESIAN_POINT ( 'NONE',  ( 18.50000000000000711, 101.5000000000000000, -1.214306433183764966E-14 ) ) ;
#1951 = ORIENTED_EDGE ( 'NONE', *, *, #5642, .F. ) ;
#1952 = ORIENTED_EDGE ( 'NONE', *, *, #1220, .T. ) ;
#1953 = DIRECTION ( 'NONE',  ( 0.000000000000000000, 0.000000000000000000, 1.000000000000000000 ) ) ;
#1954 = EDGE_CURVE ( 'NONE', #4795, #7371, #4395, .T. ) ;
#1955 = DIRECTION ( 'NONE',  ( 1.000000000000000000, 0.000000000000000000, 0.000000000000000000 ) ) ;
#1956 = LINE ( 'NONE', #1994, #5441 ) ;
#1957 = CARTESIAN_POINT ( 'NONE',  ( 50.00000000000000000, 17.91234734164656928, 13.00000000000000711 ) ) ;
#1958 = ORIENTED_EDGE ( 'NONE', *, *, #1123, .T. ) ;
#1959 = ORIENTED_EDGE ( 'NONE', *, *, #5899, .F. ) ;
#1960 = AXIS2_PLACEMENT_3D ( 'NONE', #6870, #3916, #1628 ) ;
#1961 = EDGE_CURVE ( 'NONE', #79, #7476, #2664, .T. ) ;
#1962 = CARTESIAN_POINT ( 'NONE',  ( -16.49999999999996447, 0.000000000000000000, 0.000000000000000000 ) ) ;
#1963 = FACE_OUTER_BOUND ( 'NONE', #61, .T. ) ;
#1964 = VERTEX_POINT ( 'NONE', #1807 ) ;
#1965 = EDGE_CURVE ( 'NONE', #2388, #5372, #4122, .T. ) ;
#1966 = DIRECTION ( 'NONE',  ( 0.000000000000000000, 1.156482317317871133E-15, -1.000000000000000000 ) ) ;
#1967 = CYLINDRICAL_SURFACE ( 'NONE', #431, 3.000000000000002665 ) ;
#1968 = CLOSED_SHELL ( 'NONE', ( #55, #710, #7037, #5662, #747, #795, #5068, #2514, #6814, #1629, #2500, #3511, #1862, #7189, #4176, #770, #5651, #2668, #3020, #111, #1829, #1112, #1698, #5341, #4216, #6767, #398, #5, #256, #3282, #5377, #4521, #2185, #2591, #6007, #6918, #4078, #4502, #840, #4801, #4698, #2719, #2419, #2352, #6343, #568, #6673, #537, #4376, #2565, #317, #729, #4203, #1103, #367, #2066, #2498, #1544, #5573, #3584, #610, #5510, #264, #4009, #2763, #5483, #4573, #4718, #4138, #234, #3730, #1208, #1261, #2397, #6776, #3607, #4904, #3474, #3175, #550, #5699, #1318, #5695, #4604, #3615, #3887, #7473 ) ) ;
#1969 = CIRCLE ( 'NONE', #3697, 8.500000000000007105 ) ;
#1970 = EDGE_LOOP ( 'NONE', ( #3272, #2704, #828, #807 ) ) ;
#1971 = DIRECTION ( 'NONE',  ( 1.000000000000000000, 2.465190328815661892E-32, -9.244463733058732095E-33 ) ) ;
#1972 = CARTESIAN_POINT ( 'NONE',  ( 0.000000000000000000, 0.000000000000000000, -9.999999999999994671 ) ) ;
#1973 = ORIENTED_EDGE ( 'NONE', *, *, #4742, .F. ) ;
#1974 = DIRECTION ( 'NONE',  ( -1.000000000000000000, 0.000000000000000000, -7.663350976776343357E-46 ) ) ;
#1975 = EDGE_CURVE ( 'NONE', #3162, #6147, #3043, .T. ) ;
#1976 = DIRECTION ( 'NONE',  ( 1.000000000000000000, 2.624548829666596385E-30, 9.231085635203014490E-31 ) ) ;
#1977 = EDGE_CURVE ( 'NONE', #6977, #452, #5921, .T. ) ;
#1978 = CARTESIAN_POINT ( 'NONE',  ( 24.99999999999999289, 86.00000000000001421, 4.999999999999992006 ) ) ;
#1979 = CIRCLE ( 'NONE', #6765, 10.00000000000000355 ) ;
#1980 = VERTEX_POINT ( 'NONE', #1223 ) ;
#1981 = DIRECTION ( 'NONE',  ( -1.000000000000000000, -2.624548829666596736E-30, 9.231085635203017994E-31 ) ) ;
#1982 = CARTESIAN_POINT ( 'NONE',  ( -16.50000000000000711, -214.0630240738404382, 94.50428307177961074 ) ) ;
#1983 = LINE ( 'NONE', #5027, #1657 ) ;
#1984 = CARTESIAN_POINT ( 'NONE',  ( -57.54473169771259933, -223.0630240738405234, 74.15707378103115843 ) ) ;
#1985 = ORIENTED_EDGE ( 'NONE', *, *, #327, .F. ) ;
#1986 = DIRECTION ( 'NONE',  ( -1.000000000000000000, 1.294224922628222493E-31, -1.078147950931789264E-16 ) ) ;
#1987 = CIRCLE ( 'NONE', #5552, 8.500000000000007105 ) ;
#1988 = ORIENTED_EDGE ( 'NONE', *, *, #1583, .T. ) ;
#1989 = ORIENTED_EDGE ( 'NONE', *, *, #3544, .F. ) ;
#1990 = DIRECTION ( 'NONE',  ( -4.237045877651920929E-33, -1.945189243831109306E-32, 1.000000000000000000 ) ) ;
#1991 = VECTOR ( 'NONE', #5751, 1000.000000000000000 ) ;
#1992 = FACE_OUTER_BOUND ( 'NONE', #2379, .T. ) ;
#1993 =( BOUNDED_CURVE ( )  B_SPLINE_CURVE ( 3, ( #5906, #4768, #109, #1752 ),
 .UNSPECIFIED., .F., .T. ) 
 B_SPLINE_CURVE_WITH_KNOTS ( ( 4, 4 ),
 ( 3.141592653589793116, 4.712388980384689674 ),
 .UNSPECIFIED. ) 
 CURVE ( )  GEOMETRIC_REPRESENTATION_ITEM ( )  RATIONAL_B_SPLINE_CURVE ( ( 1.000000000000000000, 0.8047378541243649375, 0.8047378541243649375, 1.000000000000000000 ) ) 
 REPRESENTATION_ITEM ( '' )  );
#1994 = CARTESIAN_POINT ( 'NONE',  ( -13.64230087749234599, 16.00000000000004263, 38.63670350735201708 ) ) ;
#1995 =( NAMED_UNIT ( * ) SI_UNIT ( $, .STERADIAN. ) SOLID_ANGLE_UNIT ( ) );
#1996 = CARTESIAN_POINT ( 'NONE',  ( -63.67592485445254624, -218.0630209448846699, 88.03053438521520491 ) ) ;
#1997 = VERTEX_POINT ( 'NONE', #3582 ) ;
#1998 = EDGE_CURVE ( 'NONE', #1936, #7257, #1069, .T. ) ;
#1999 = ORIENTED_EDGE ( 'NONE', *, *, #4689, .F. ) ;
#2000 = AXIS2_PLACEMENT_3D ( 'NONE', #5367, #5207, #1858 ) ;
#2001 = LINE ( 'NONE', #6808, #7182 ) ;
#2002 = CARTESIAN_POINT ( 'NONE',  ( 27.03121585365657609, -225.8512969706634124, 79.74927943323393720 ) ) ;
#2003 = ORIENTED_EDGE ( 'NONE', *, *, #3395, .F. ) ;
#2004 = DIRECTION ( 'NONE',  ( 1.000000000000000000, 0.000000000000000000, 7.663350976776343357E-46 ) ) ;
#2005 = DIRECTION ( 'NONE',  ( -1.000000000000000000, 1.294224922628222493E-31, -1.078147950931789757E-16 ) ) ;
#2006 = ORIENTED_EDGE ( 'NONE', *, *, #3422, .F. ) ;
#2007 = EDGE_CURVE ( 'NONE', #4921, #6198, #6353, .T. ) ;
#2008 = CIRCLE ( 'NONE', #1508, 6.000000000000003553 ) ;
#2009 = CYLINDRICAL_SURFACE ( 'NONE', #2551, 7.999999999999986677 ) ;
#2010 = CARTESIAN_POINT ( 'NONE',  ( 52.24271833150618960, 27.04204335853172836, 10.00000000000000888 ) ) ;
#2011 = LINE ( 'NONE', #4945, #6075 ) ;
#2012 = ORIENTED_EDGE ( 'NONE', *, *, #40, .F. ) ;
#2013 = CARTESIAN_POINT ( 'NONE',  ( 53.00000000000000711, 24.00878702352406435, 10.00000000000001066 ) ) ;
#2014 = COLOUR_RGB ( '',0.7921568627450980005, 0.8196078431372548767, 0.9333333333333333481 ) ;
#2015 = FACE_OUTER_BOUND ( 'NONE', #1221, .T. ) ;
#2016 = SURFACE_STYLE_USAGE ( .BOTH. , #6020 ) ;
#2017 = EDGE_LOOP ( 'NONE', ( #3414, #5671, #2424, #3659 ) ) ;
#2018 = VECTOR ( 'NONE', #2237, 1000.000000000000000 ) ;
#2019 = AXIS2_PLACEMENT_3D ( 'NONE', #1972, #6560, #5406 ) ;
#2020 = ADVANCED_FACE ( 'NONE', ( #33 ), #5272, .T. ) ;
#2021 = CIRCLE ( 'NONE', #6940, 3.000000000000000444 ) ;
#2022 = DIRECTION ( 'NONE',  ( 1.000000000000000000, 0.000000000000000000, 0.000000000000000000 ) ) ;
#2023 =( NAMED_UNIT ( * ) SI_UNIT ( $, .STERADIAN. ) SOLID_ANGLE_UNIT ( ) );
#2024 = DIRECTION ( 'NONE',  ( -1.000000000000000000, 5.551115123125783935E-17, -4.237045877651919561E-33 ) ) ;
#2025 = CARTESIAN_POINT ( 'NONE',  ( -54.69181398302472275, -223.0639029778887448, 73.35099609428758072 ) ) ;
#2026 = DIRECTION ( 'NONE',  ( 1.000000000000000000, 0.000000000000000000, 0.000000000000000000 ) ) ;
#2027 = CARTESIAN_POINT ( 'NONE',  ( 220.0000000000000000, 20.99999999999999645, 10.00000000000001066 ) ) ;
#2028 = AXIS2_PLACEMENT_3D ( 'NONE', #4346, #3847, #7375 ) ;
#2029 = CIRCLE ( 'NONE', #188, 9.999999999999998224 ) ;
#2030 = VECTOR ( 'NONE', #3418, 1000.000000000000000 ) ;
#2031 = ORIENTED_EDGE ( 'NONE', *, *, #2807, .T. ) ;
#2032 = EDGE_CURVE ( 'NONE', #5020, #5755, #3662, .T. ) ;
#2033 = ORIENTED_EDGE ( 'NONE', *, *, #3720, .T. ) ;
#2034 = PRODUCT_DEFINITION_FORMATION_WITH_SPECIFIED_SOURCE ( 'ANY', '', #5056, .NOT_KNOWN. ) ;
#2035 = FACE_OUTER_BOUND ( 'NONE', #3316, .T. ) ;
#2036 = CARTESIAN_POINT ( 'NONE',  ( 24.99999999999998579, 101.4999999999999858, -1.734723475976807094E-15 ) ) ;
#2037 = LINE ( 'NONE', #6143, #2365 ) ;
#2038 = PLANE ( 'NONE',  #819 ) ;
#2039 = ORIENTED_EDGE ( 'NONE', *, *, #6512, .F. ) ;
#2040 = VERTEX_POINT ( 'NONE', #1075 ) ;
#2041 = ORIENTED_EDGE ( 'NONE', *, *, #6801, .T. ) ;
#2042 = EDGE_CURVE ( 'NONE', #2908, #1843, #6367, .T. ) ;
#2043 = FACE_OUTER_BOUND ( 'NONE', #5010, .T. ) ;
#2044 = PLANE ( 'NONE',  #7188 ) ;
#2045 = ORIENTED_EDGE ( 'NONE', *, *, #1360, .T. ) ;
#2046 = CIRCLE ( 'NONE', #4642, 7.999999999999992895 ) ;
#2047 = CARTESIAN_POINT ( 'NONE',  ( -32.50000000000002842, -49.37258300203047412, 0.000000000000000000 ) ) ;
#2048 = LINE ( 'NONE', #7280, #4234 ) ;
#2049 = CARTESIAN_POINT ( 'NONE',  ( 202.0000000000000568, -10.95994505756729254, 7.000000000000021316 ) ) ;
#2050 = ORIENTED_EDGE ( 'NONE', *, *, #4653, .F. ) ;
#2051 = AXIS2_PLACEMENT_3D ( 'NONE', #1707, #1745, #1671 ) ;
#2052 = ADVANCED_FACE ( 'NONE', ( #6504 ), #6389, .F. ) ;
#2053 = CARTESIAN_POINT ( 'NONE',  ( 185.0000000000000000, 39.99999999999999289, 0.000000000000000000 ) ) ;
#2054 = FACE_OUTER_BOUND ( 'NONE', #3481, .T. ) ;
#2055 = CARTESIAN_POINT ( 'NONE',  ( 10.25168462842736261, -218.0630240738404950, 95.20959099461346398 ) ) ;
#2056 = VERTEX_POINT ( 'NONE', #5772 ) ;
#2057 = ORIENTED_EDGE ( 'NONE', *, *, #7168, .T. ) ;
#2058 = AXIS2_PLACEMENT_3D ( 'NONE', #531, #6427, #4628 ) ;
#2059 =( REPRESENTATION_RELATIONSHIP ('NONE','NONE', #4862, #915 ) REPRESENTATION_RELATIONSHIP_WITH_TRANSFORMATION ( #1738 )SHAPE_REPRESENTATION_RELATIONSHIP( ) );
#2060 = DIRECTION ( 'NONE',  ( -1.000000000000000000, -0.000000000000000000, -0.000000000000000000 ) ) ;
#2061 = CARTESIAN_POINT ( 'NONE',  ( 200.0000000000000000, 0.000000000000000000, 0.000000000000000000 ) ) ;
#2062 = CARTESIAN_POINT ( 'NONE',  ( 50.00000000000001421, 15.08392021690038121, 12.00000000000000711 ) ) ;
#2063 = CARTESIAN_POINT ( 'NONE',  ( -61.64566566670315240, -223.0630240738406371, 77.11548722274392276 ) ) ;
#2064 = CARTESIAN_POINT ( 'NONE',  ( 0.000000000000000000, 0.000000000000000000, -3.000000000000002665 ) ) ;
#2065 = CARTESIAN_POINT ( 'NONE',  ( 50.00000000000000000, 4.543323389463065786E-15, 13.00000000000001066 ) ) ;
#2066 = ADVANCED_FACE ( 'NONE', ( #2884 ), #494, .T. ) ;
#2067 = B_SPLINE_CURVE_WITH_KNOTS ( 'NONE', 3,
 ( #4652, #6215, #3298, #5640, #3376, #2749 ),
 .UNSPECIFIED., .F., .F.,
 ( 4, 2, 4 ),
 ( 0.000000000000000000, 0.002568044547241824134, 0.005136089094483648268 ),
 .UNSPECIFIED. ) ;
#2068 = ORIENTED_EDGE ( 'NONE', *, *, #3483, .T. ) ;
#2069 = VERTEX_POINT ( 'NONE', #2421 ) ;
#2070 = CARTESIAN_POINT ( 'NONE',  ( 220.0000000000000000, -20.99999999999999645, 13.00000000000000888 ) ) ;
#2071 = LINE ( 'NONE', #3112, #3386 ) ;
#2072 = PLANE ( 'NONE',  #5922 ) ;
#2073 = EDGE_CURVE ( 'NONE', #908, #472, #2429, .T. ) ;
#2074 = B_SPLINE_CURVE_WITH_KNOTS ( 'NONE', 3,
 ( #6711, #856, #1580, #3445, #6860, #3979 ),
 .UNSPECIFIED., .F., .F.,
 ( 4, 2, 4 ),
 ( 0.000000000000000000, 0.002568044547241839747, 0.005136089094483679493 ),
 .UNSPECIFIED. ) ;
#2075 = EDGE_CURVE ( 'NONE', #2971, #2880, #6728, .T. ) ;
#2076 = ORIENTED_EDGE ( 'NONE', *, *, #5509, .F. ) ;
#2077 = ORIENTED_EDGE ( 'NONE', *, *, #6933, .T. ) ;
#2078 = CARTESIAN_POINT ( 'NONE',  ( 50.01335591787554335, -18.01335591787552559, 12.66922467357069593 ) ) ;
#2079 = EDGE_LOOP ( 'NONE', ( #5041, #1021, #372, #440 ) ) ;
#2080 = CARTESIAN_POINT ( 'NONE',  ( 217.0000000000000000, -20.99999999999999645, 13.00000000000000888 ) ) ;
#2081 = DIRECTION ( 'NONE',  ( -1.000000000000000000, 0.000000000000000000, -7.663350976776343357E-46 ) ) ;
#2082 = ORIENTED_EDGE ( 'NONE', *, *, #1690, .F. ) ;
#2083 = B_SPLINE_CURVE_WITH_KNOTS ( 'NONE', 3,
 ( #2306, #1834, #602, #4076, #5299, #4806, #4157, #6421, #7144, #1873, #3073, #28 ),
 .UNSPECIFIED., .F., .F.,
 ( 4, 2, 2, 2, 2, 4 ),
 ( 0.000000000000000000, 0.001107519046781883440, 0.002215038093563766880, 0.003322557140345648152, 0.003876316663736585968, 0.004430076187127524219 ),
 .UNSPECIFIED. ) ;
#2084 =( GEOMETRIC_REPRESENTATION_CONTEXT ( 3 ) GLOBAL_UNCERTAINTY_ASSIGNED_CONTEXT ( ( #1251 ) ) GLOBAL_UNIT_ASSIGNED_CONTEXT ( ( #4876, #5601, #325 ) ) REPRESENTATION_CONTEXT ( 'NONE', 'WORKASPACE' ) );
#2085 = DIRECTION ( 'NONE',  ( 1.000000000000000000, 0.000000000000000000, 7.663350976776343357E-46 ) ) ;
#2086 = CARTESIAN_POINT ( 'NONE',  ( -14.65391489814400572, -111.4855484589742360, 39.48554845897440657 ) ) ;
#2087 = CYLINDRICAL_SURFACE ( 'NONE', #3872, 6.000000000000003553 ) ;
#2088 = ORIENTED_EDGE ( 'NONE', *, *, #3608, .F. ) ;
#2089 = CARTESIAN_POINT ( 'NONE',  ( -53.00237955168282866, -212.4343899438498795, 94.21711093295959927 ) ) ;
#2090 = CLOSED_SHELL ( 'NONE', ( #2904, #4938, #3218, #6795, #1530, #5222, #5447, #286, #2729, #7031, #3531, #1761, #6303, #5149 ) ) ;
#2091 = DIRECTION ( 'NONE',  ( -1.000000000000000000, -2.465190328815661892E-32, 9.244463733058732095E-33 ) ) ;
#2092 = VECTOR ( 'NONE', #3766, 1000.000000000000000 ) ;
#2093 = DIRECTION ( 'NONE',  ( -1.000000000000000000, -0.000000000000000000, -0.000000000000000000 ) ) ;
#2094 = ORIENTED_EDGE ( 'NONE', *, *, #5015, .T. ) ;
#2095 = EDGE_CURVE ( 'NONE', #3503, #4666, #4613, .T. ) ;
#2096 = DIRECTION ( 'NONE',  ( 0.7071067811865462405, 8.659560562354950115E-17, 0.7071067811865489050 ) ) ;
#2097 = DIRECTION ( 'NONE',  ( 1.000000000000000000, 1.853902270198408060E-44, 1.681558157189780485E-44 ) ) ;
#2098 = CARTESIAN_POINT ( 'NONE',  ( 191.1899843872966471, 6.079033463187697883, 17.21004863381197936 ) ) ;
#2099 = FACE_OUTER_BOUND ( 'NONE', #5489, .T. ) ;
#2100 = CARTESIAN_POINT ( 'NONE',  ( 186.9059892324150383, -5.031373033403107264, 15.00000000000000888 ) ) ;
#2101 = LINE ( 'NONE', #3107, #7370 ) ;
#2102 = ORIENTED_EDGE ( 'NONE', *, *, #1965, .T. ) ;
#2103 = ADVANCED_FACE ( 'NONE', ( #2277 ), #5852, .T. ) ;
#2104 = ORIENTED_EDGE ( 'NONE', *, *, #3061, .T. ) ;
#2105 = CARTESIAN_POINT ( 'NONE',  ( -10.49999999999997513, -39.68629150101520509, 23.99999999999999289 ) ) ;
#2106 = CARTESIAN_POINT ( 'NONE',  ( 217.0000000000000000, 0.000000000000000000, 12.00000000000000711 ) ) ;
#2107 = LINE ( 'NONE', #339, #6072 ) ;
#2108 = CARTESIAN_POINT ( 'NONE',  ( 26.00000000000000000, 0.000000000000000000, 0.000000000000000000 ) ) ;
#2109 = AXIS2_PLACEMENT_3D ( 'NONE', #744, #5448, #3646 ) ;
#2110 = ORIENTED_EDGE ( 'NONE', *, *, #4377, .F. ) ;
#2111 = VERTEX_POINT ( 'NONE', #7572 ) ;
#2112 = CIRCLE ( 'NONE', #30, 6.000000000000000888 ) ;
#2113 = ADVANCED_FACE ( 'NONE', ( #3545, #4664, #1725 ), #607, .F. ) ;
#2114 = EDGE_CURVE ( 'NONE', #551, #3791, #688, .T. ) ;
#2115 = DIRECTION ( 'NONE',  ( 1.000000000000000000, 0.000000000000000000, 7.663350976776343357E-46 ) ) ;
#2116 = VERTEX_POINT ( 'NONE', #3770 ) ;
#2117 = DIRECTION ( 'NONE',  ( -5.551115123125785167E-17, 0.7071067811865469066, 0.7071067811865482389 ) ) ;
#2118 = LINE ( 'NONE', #3969, #4000 ) ;
#2119 = ORIENTED_EDGE ( 'NONE', *, *, #7417, .F. ) ;
#2120 = EDGE_CURVE ( 'NONE', #6255, #2955, #5426, .T. ) ;
#2121 = CARTESIAN_POINT ( 'NONE',  ( 189.5040654437683258, 3.000000000000000000, 19.50000000000000711 ) ) ;
#2122 = DIRECTION ( 'NONE',  ( 1.000000000000000000, 0.000000000000000000, 0.000000000000000000 ) ) ;
#2123 = ORIENTED_EDGE ( 'NONE', *, *, #1430, .T. ) ;
#2124 = DIRECTION ( 'NONE',  ( 1.000000000000000000, 2.465190328815661892E-32, -9.244463733058732095E-33 ) ) ;
#2125 = CYLINDRICAL_SURFACE ( 'NONE', #2706, 2.999999999999999112 ) ;
#2126 = DIRECTION ( 'NONE',  ( 1.000000000000000000, 0.000000000000000000, 0.000000000000000000 ) ) ;
#2127 = ORIENTED_EDGE ( 'NONE', *, *, #1360, .F. ) ;
#2128 = ORIENTED_EDGE ( 'NONE', *, *, #3493, .F. ) ;
#2129 = DIRECTION ( 'NONE',  ( 0.000000000000000000, 0.000000000000000000, -1.000000000000000000 ) ) ;
#2130 = AXIS2_PLACEMENT_3D ( 'NONE', #1116, #5198, #4127 ) ;
#2131 = AXIS2_PLACEMENT_3D ( 'NONE', #5342, #7071, #5995 ) ;
#2132 = LINE ( 'NONE', #5674, #4242 ) ;
#2133 = CARTESIAN_POINT ( 'NONE',  ( 188.6381938907515519, 9.028273915299429575, 15.00013323867315940 ) ) ;
#2134 = CYLINDRICAL_SURFACE ( 'NONE', #1886, 15.99999999999997335 ) ;
#2135 = CARTESIAN_POINT ( 'NONE',  ( 209.9999999999999716, -6.000000000000000000, 35.00000000000000000 ) ) ;
#2136 = DIRECTION ( 'NONE',  ( 9.231085635203014490E-31, 0.000000000000000000, -1.000000000000000000 ) ) ;
#2137 = EDGE_CURVE ( 'NONE', #6069, #1494, #6110, .T. ) ;
#2138 = CARTESIAN_POINT ( 'NONE',  ( -57.71305776231798745, -218.0630565819627122, 72.97053707171922099 ) ) ;
#2139 = EDGE_CURVE ( 'NONE', #3264, #441, #1335, .T. ) ;
#2140 = VECTOR ( 'NONE', #7433, 1000.000000000000000 ) ;
#2141 = AXIS2_PLACEMENT_3D ( 'NONE', #1432, #3205, #5129 ) ;
#2142 = EDGE_LOOP ( 'NONE', ( #7174, #4482 ) ) ;
#2143 = ORIENTED_EDGE ( 'NONE', *, *, #4275, .T. ) ;
#2144 = DIRECTION ( 'NONE',  ( 1.000000000000000000, -0.000000000000000000, 0.000000000000000000 ) ) ;
#2145 = LINE ( 'NONE', #5006, #1804 ) ;
#2146 = AXIS2_PLACEMENT_3D ( 'NONE', #808, #205, #3159 ) ;
#2147 = DIRECTION ( 'NONE',  ( 1.000000000000000000, 1.853902270198408060E-44, 1.681558157189780485E-44 ) ) ;
#2148 = FACE_OUTER_BOUND ( 'NONE', #5700, .T. ) ;
#2149 = AXIS2_PLACEMENT_3D ( 'NONE', #59, #7020, #6486 ) ;
#2150 = VECTOR ( 'NONE', #4030, 1000.000000000000000 ) ;
#2151 = CARTESIAN_POINT ( 'NONE',  ( -24.00000000000000000, 3.122849337825749433E-15, -1.540743955509789033E-30 ) ) ;
#2152 = ADVANCED_FACE ( 'NONE', ( #4888 ), #6687, .F. ) ;
#2153 = ORIENTED_EDGE ( 'NONE', *, *, #3745, .F. ) ;
#2154 = PRODUCT_DEFINITION_FORMATION_WITH_SPECIFIED_SOURCE ( 'ANY', '', #2227, .NOT_KNOWN. ) ;
#2155 = VERTEX_POINT ( 'NONE', #7150 ) ;
#2156 = DIRECTION ( 'NONE',  ( 1.000000000000000000, 2.465190328815661892E-32, -9.244463733058732095E-33 ) ) ;
#2157 = ORIENTED_EDGE ( 'NONE', *, *, #406, .T. ) ;
#2158 = CARTESIAN_POINT ( 'NONE',  ( 52.24271833151664168, -25.80522265072890420, 10.00000000000000888 ) ) ;
#2159 = DIRECTION ( 'NONE',  ( 1.000000000000000000, 0.000000000000000000, 0.000000000000000000 ) ) ;
#2160 = PRODUCT ( 'MAT-051', 'MAT-051', '', ( #4792 ) ) ;
#2161 = EDGE_CURVE ( 'NONE', #7239, #4415, #4271, .T. ) ;
#2162 =( REPRESENTATION_RELATIONSHIP ('NONE','NONE', #4862, #97 ) REPRESENTATION_RELATIONSHIP_WITH_TRANSFORMATION ( #7047 )SHAPE_REPRESENTATION_RELATIONSHIP( ) );
#2163 = VERTEX_POINT ( 'NONE', #801 ) ;
#2164 = LINE ( 'NONE', #4672, #7051 ) ;
#2165 = LINE ( 'NONE', #1538, #5589 ) ;
#2166 = ORIENTED_EDGE ( 'NONE', *, *, #483, .T. ) ;
#2167 = CARTESIAN_POINT ( 'NONE',  ( 210.0000000000002274, 20.50000000000002132, 34.99999999999842970 ) ) ;
#2168 = CARTESIAN_POINT ( 'NONE',  ( -69.99871551551754578, -224.9174535703052413, 90.83998408137780700 ) ) ;
#2169 = DIRECTION ( 'NONE',  ( -0.000000000000000000, -1.000000000000000000, -0.000000000000000000 ) ) ;
#2170 = LINE ( 'NONE', #3908, #2262 ) ;
#2171 = AXIS2_PLACEMENT_3D ( 'NONE', #4656, #1755, #1178 ) ;
#2172 = VERTEX_POINT ( 'NONE', #1840 ) ;
#2173 = ADVANCED_FACE ( 'NONE', ( #7191, #3042 ), #7116, .F. ) ;
#2174 = VERTEX_POINT ( 'NONE', #1416 ) ;
#2175 = AXIS2_PLACEMENT_3D ( 'NONE', #6531, #3723, #3031 ) ;
#2176 = CARTESIAN_POINT ( 'NONE',  ( 220.0000000000000000, 18.00000000000000000, 15.00000000000000888 ) ) ;
#2177 = CARTESIAN_POINT ( 'NONE',  ( 186.9061174410084334, 9.037698274678149346, 15.00022206379774659 ) ) ;
#2178 = CARTESIAN_POINT ( 'NONE',  ( -63.72797457321117776, -223.0630240738404950, 88.96157793287162008 ) ) ;
#2179 = DIRECTION ( 'NONE',  ( 0.000000000000000000, 1.000000000000000000, 0.000000000000000000 ) ) ;
#2180 = CARTESIAN_POINT ( 'NONE',  ( -26.49999999999999645, -214.0630240738404666, 70.86973541144037370 ) ) ;
#2181 = CARTESIAN_POINT ( 'NONE',  ( -61.17656753709511008, -218.0630265158296481, 75.43246580923499778 ) ) ;
#2182 = VECTOR ( 'NONE', #6740, 1000.000000000000000 ) ;
#2183 = VERTEX_POINT ( 'NONE', #1302 ) ;
#2184 = ORIENTED_EDGE ( 'NONE', *, *, #1598, .T. ) ;
#2185 = ADVANCED_FACE ( 'NONE', ( #1920 ), #6000, .T. ) ;
#2186 = DIRECTION ( 'NONE',  ( -1.853902270198407313E-44, -1.000000000000000000, 0.000000000000000000 ) ) ;
#2187 = DIRECTION ( 'NONE',  ( 0.000000000000000000, 0.000000000000000000, -1.000000000000000000 ) ) ;
#2188 = LINE ( 'NONE', #4540, #7065 ) ;
#2189 = CARTESIAN_POINT ( 'NONE',  ( 2.000000000000001776, -4.163336342344337027E-14, -9.999999999999998224 ) ) ;
#2190 = FACE_OUTER_BOUND ( 'NONE', #1539, .T. ) ;
#2191 = ORIENTED_EDGE ( 'NONE', *, *, #4675, .F. ) ;
#2192 = VERTEX_POINT ( 'NONE', #119 ) ;
#2193 = CARTESIAN_POINT ( 'NONE',  ( 185.0000000000000000, 39.99999999999999289, 0.000000000000000000 ) ) ;
#2194 = ORIENTED_EDGE ( 'NONE', *, *, #6096, .F. ) ;
#2195 = DIRECTION ( 'NONE',  ( 1.000000000000000000, -0.000000000000000000, -0.000000000000000000 ) ) ;
#2196 = CARTESIAN_POINT ( 'NONE',  ( 193.5000000000000000, -39.99999999999999289, 10.00000000000000355 ) ) ;
#2197 =( BOUNDED_CURVE ( )  B_SPLINE_CURVE ( 3, ( #4396, #5511, #6697, #4428 ),
 .UNSPECIFIED., .F., .T. ) 
 B_SPLINE_CURVE_WITH_KNOTS ( ( 4, 4 ),
 ( 4.712388980384690562, 6.283185307179586232 ),
 .UNSPECIFIED. ) 
 CURVE ( )  GEOMETRIC_REPRESENTATION_ITEM ( )  RATIONAL_B_SPLINE_CURVE ( ( 1.000000000000000000, 0.8047378541243652705, 0.8047378541243652705, 1.000000000000000000 ) ) 
 REPRESENTATION_ITEM ( '' )  );
#2198 = ORIENTED_EDGE ( 'NONE', *, *, #5673, .T. ) ;
#2199 = EDGE_CURVE ( 'NONE', #7371, #7274, #1370, .T. ) ;
#2200 = EDGE_CURVE ( 'NONE', #5737, #2726, #229, .T. ) ;
#2201 = FACE_OUTER_BOUND ( 'NONE', #5246, .T. ) ;
#2202 = CARTESIAN_POINT ( 'NONE',  ( 26.00000000000000000, 0.000000000000000000, 0.000000000000000000 ) ) ;
#2203 = ORIENTED_EDGE ( 'NONE', *, *, #7493, .F. ) ;
#2204 =( NAMED_UNIT ( * ) SI_UNIT ( $, .STERADIAN. ) SOLID_ANGLE_UNIT ( ) );
#2205 = DIRECTION ( 'NONE',  ( 0.000000000000000000, 0.000000000000000000, 1.000000000000000000 ) ) ;
#2206 = DIRECTION ( 'NONE',  ( -1.000000000000000000, 5.551115123125783935E-17, -4.237045877651919561E-33 ) ) ;
#2207 = DIRECTION ( 'NONE',  ( -0.000000000000000000, 1.000000000000000000, 3.304235192336776498E-16 ) ) ;
#2208 =( REPRESENTATION_RELATIONSHIP ('NONE','NONE', #4862, #7252 ) REPRESENTATION_RELATIONSHIP_WITH_TRANSFORMATION ( #4900 )SHAPE_REPRESENTATION_RELATIONSHIP( ) );
#2209 = ORIENTED_EDGE ( 'NONE', *, *, #1070, .F. ) ;
#2210 = ORIENTED_EDGE ( 'NONE', *, *, #7556, .F. ) ;
#2211 = DIRECTION ( 'NONE',  ( 0.000000000000000000, 0.000000000000000000, -1.000000000000000000 ) ) ;
#2212 = AXIS2_PLACEMENT_3D ( 'NONE', #64, #711, #3682 ) ;
#2213 = EDGE_CURVE ( 'NONE', #2502, #5322, #5612, .T. ) ;
#2214 = DIRECTION ( 'NONE',  ( -1.000000000000000000, 5.551115123125783935E-17, -4.237045877651919561E-33 ) ) ;
#2215 = EDGE_CURVE ( 'NONE', #1645, #2264, #2984, .T. ) ;
#2216 = CIRCLE ( 'NONE', #4302, 3.000000000000000000 ) ;
#2217 = CARTESIAN_POINT ( 'NONE',  ( -16.49999999999999289, -120.9522879036832848, 45.92078884797942351 ) ) ;
#2218 = CARTESIAN_POINT ( 'NONE',  ( -57.80716452887639178, -223.0630240738405803, 95.18803987619344298 ) ) ;
#2219 = CARTESIAN_POINT ( 'NONE',  ( 15.12446775957286604, -223.0630240738405234, 95.04560220544016147 ) ) ;
#2220 = CARTESIAN_POINT ( 'NONE',  ( 47.00000000000000000, 27.04312195450891565, 12.73853277175702559 ) ) ;
#2221 = CARTESIAN_POINT ( 'NONE',  ( -62.88741732078067770, -218.0636600088369050, 77.64984730018771586 ) ) ;
#2222 = AXIS2_PLACEMENT_3D ( 'NONE', #1239, #3708, #5975 ) ;
#2223 = ORIENTED_EDGE ( 'NONE', *, *, #6269, .F. ) ;
#2224 = ORIENTED_EDGE ( 'NONE', *, *, #6620, .F. ) ;
#2225 = DIRECTION ( 'NONE',  ( 1.000000000000000000, -0.000000000000000000, -0.000000000000000000 ) ) ;
#2226 = LINE ( 'NONE', #5297, #1422 ) ;
#2227 = PRODUCT ( 'small revit', 'small revit', '', ( #6516 ) ) ;
#2228 = DIRECTION ( 'NONE',  ( 1.000000000000000000, 0.000000000000000000, 0.000000000000000000 ) ) ;
#2229 = CARTESIAN_POINT ( 'NONE',  ( 217.0000000000000000, 15.08392021690038121, 12.00000000000000711 ) ) ;
#2230 = VECTOR ( 'NONE', #6896, 1000.000000000000000 ) ;
#2231 = DIRECTION ( 'NONE',  ( -1.000000000000000000, 0.000000000000000000, 0.000000000000000000 ) ) ;
#2232 = EDGE_LOOP ( 'NONE', ( #94, #298, #2657, #6478 ) ) ;
#2233 = AXIS2_PLACEMENT_3D ( 'NONE', #4868, #50, #7093 ) ;
#2234 = ORIENTED_EDGE ( 'NONE', *, *, #1908, .T. ) ;
#2235 = DIRECTION ( 'NONE',  ( 4.622231866529368100E-33, -2.600005424922769496E-32, 1.000000000000000000 ) ) ;
#2236 = VECTOR ( 'NONE', #4298, 1000.000000000000114 ) ;
#2237 = DIRECTION ( 'NONE',  ( 0.000000000000000000, -1.000000000000000000, 0.000000000000000000 ) ) ;
#2238 = VERTEX_POINT ( 'NONE', #5962 ) ;
#2239 = PRODUCT ( 'socket', 'socket', '', ( #5283 ) ) ;
#2240 = DIRECTION ( 'NONE',  ( -2.465190328815661892E-32, -0.7071067811865465735, 0.7071067811865484609 ) ) ;
#2241 = ADVANCED_FACE ( 'NONE', ( #1262 ), #3620, .T. ) ;
#2242 = ORIENTED_EDGE ( 'NONE', *, *, #1143, .F. ) ;
#2243 = AXIS2_PLACEMENT_3D ( 'NONE', #7213, #4908, #5407 ) ;
#2244 = ORIENTED_EDGE ( 'NONE', *, *, #6586, .F. ) ;
#2245 = DIRECTION ( 'NONE',  ( -1.000000000000000000, 0.000000000000000000, -7.663350976776343357E-46 ) ) ;
#2246 = CARTESIAN_POINT ( 'NONE',  ( 17.70193531918452123, -214.7694783647498866, 94.62885002390537181 ) ) ;
#2247 = ORIENTED_EDGE ( 'NONE', *, *, #4075, .T. ) ;
#2248 = DIRECTION ( 'NONE',  ( 0.000000000000000000, 0.000000000000000000, 1.000000000000000000 ) ) ;
#2249 = CARTESIAN_POINT ( 'NONE',  ( -60.68960140267979853, -213.9340789708222133, 94.48154657109718357 ) ) ;
#2250 = DIRECTION ( 'NONE',  ( -0.000000000000000000, 0.000000000000000000, -1.000000000000000000 ) ) ;
#2251 = DIRECTION ( 'NONE',  ( 4.622231866529368100E-33, -2.600005424922769496E-32, 1.000000000000000000 ) ) ;
#2252 = EDGE_CURVE ( 'NONE', #7513, #3412, #1503, .T. ) ;
#2253 = ORIENTED_EDGE ( 'NONE', *, *, #875, .T. ) ;
#2254 = ORIENTED_EDGE ( 'NONE', *, *, #6378, .T. ) ;
#2255 = DIRECTION ( 'NONE',  ( 2.627434620609032786E-46, -0.9659258262890683122, 0.2588190451025207950 ) ) ;
#2256 = CARTESIAN_POINT ( 'NONE',  ( 186.0358176304254698, 8.266324145821753788, 13.49281857405051355 ) ) ;
#2257 = DIRECTION ( 'NONE',  ( 1.445602896647337931E-16, -0.000000000000000000, 1.000000000000000000 ) ) ;
#2258 = CARTESIAN_POINT ( 'NONE',  ( 2.775557561562891351E-14, 86.00000000000000000, -1.387778780781445676E-14 ) ) ;
#2259 = DIRECTION ( 'NONE',  ( 1.000000000000000000, 0.000000000000000000, 0.000000000000000000 ) ) ;
#2260 = CARTESIAN_POINT ( 'NONE',  ( -64.50055673519366906, -218.0630240738405803, 83.63996444840225308 ) ) ;
#2261 = EDGE_CURVE ( 'NONE', #1241, #6856, #6876, .T. ) ;
#2262 = VECTOR ( 'NONE', #439, 1000.000000000000000 ) ;
#2263 = CIRCLE ( 'NONE', #2383, 6.000000000000000000 ) ;
#2264 = VERTEX_POINT ( 'NONE', #3385 ) ;
#2265 = CARTESIAN_POINT ( 'NONE',  ( 35.00000000000000000, 39.99999999999999289, 10.00000000000000355 ) ) ;
#2266 = DIRECTION ( 'NONE',  ( 0.000000000000000000, 0.000000000000000000, -1.000000000000000000 ) ) ;
#2267 = DIRECTION ( 'NONE',  ( 0.000000000000000000, 0.08715574274766231533, -0.9961946980917453232 ) ) ;
#2268 = DIRECTION ( 'NONE',  ( -1.000000000000000000, -0.000000000000000000, -0.000000000000000000 ) ) ;
#2269 = CARTESIAN_POINT ( 'NONE',  ( 186.9059892324694943, -8.476231918229933271, 15.00000000001430323 ) ) ;
#2270 = VECTOR ( 'NONE', #1194, 1000.000000000000000 ) ;
#2271 = MECHANICAL_DESIGN_GEOMETRIC_PRESENTATION_REPRESENTATION (  '', ( #5582 ), #3865 ) ;
#2272 = EDGE_CURVE ( 'NONE', #4080, #1754, #2145, .T. ) ;
#2273 = ORIENTED_EDGE ( 'NONE', *, *, #2332, .T. ) ;
#2274 = EDGE_LOOP ( 'NONE', ( #2930, #6780 ) ) ;
#2275 = VECTOR ( 'NONE', #5813, 1000.000000000000000 ) ;
#2276 = AXIS2_PLACEMENT_3D ( 'NONE', #3724, #2097, #6210 ) ;
#2277 = FACE_OUTER_BOUND ( 'NONE', #4409, .T. ) ;
#2278 = CARTESIAN_POINT ( 'NONE',  ( 17.99999999999999645, 0.000000000000000000, -39.99999999999997868 ) ) ;
#2279 = VERTEX_POINT ( 'NONE', #910 ) ;
#2280 = DIRECTION ( 'NONE',  ( -0.000000000000000000, -0.000000000000000000, 1.000000000000000000 ) ) ;
#2281 = VECTOR ( 'NONE', #3930, 1000.000000000000000 ) ;
#2282 = VECTOR ( 'NONE', #6535, 1000.000000000000000 ) ;
#2283 = ORIENTED_EDGE ( 'NONE', *, *, #271, .T. ) ;
#2284 = VERTEX_POINT ( 'NONE', #4500 ) ;
#2285 = EDGE_CURVE ( 'NONE', #6005, #6273, #6099, .T. ) ;
#2286 = CARTESIAN_POINT ( 'NONE',  ( 25.00000000000002132, 73.78679656440357348, 0.9999999999999991118 ) ) ;
#2287 = CARTESIAN_POINT ( 'NONE',  ( 10.50256896896191527, -223.7273137069649067, 96.20835808348054741 ) ) ;
#2288 = AXIS2_PLACEMENT_3D ( 'NONE', #4475, #6936, #3905 ) ;
#2289 = ORIENTED_EDGE ( 'NONE', *, *, #5955, .T. ) ;
#2290 = PRODUCT_CONTEXT ( 'NONE', #204, 'mechanical' ) ;
#2291 = CARTESIAN_POINT ( 'NONE',  ( 0.000000000000000000, 0.000000000000000000, 35.00000000000000000 ) ) ;
#2292 = SPHERICAL_SURFACE ( 'NONE', #2496, 3.000000000000000000 ) ;
#2293 = EDGE_LOOP ( 'NONE', ( #1148, #5238, #2694, #351, #4930, #657, #6278 ) ) ;
#2294 = EDGE_LOOP ( 'NONE', ( #6663, #4137 ) ) ;
#2295 = CARTESIAN_POINT ( 'NONE',  ( -19.15685424949237969, 16.00000000000004263, 36.65685424949246851 ) ) ;
#2296 = DIRECTION ( 'NONE',  ( 0.7071067811865514585, 0.000000000000000000, -0.7071067811865435759 ) ) ;
#2297 = AXIS2_PLACEMENT_3D ( 'NONE', #5876, #5151, #6459 ) ;
#2298 =( NAMED_UNIT ( * ) SI_UNIT ( $, .STERADIAN. ) SOLID_ANGLE_UNIT ( ) );
#2299 = CARTESIAN_POINT ( 'NONE',  ( 20.08074261902346791, -218.0630240738405519, 89.32155595708078977 ) ) ;
#2300 = CARTESIAN_POINT ( 'NONE',  ( 14.39358511678551089, -223.0630240738404098, 74.09254973739808747 ) ) ;
#2301 = CARTESIAN_POINT ( 'NONE',  ( 4.000000000000000000, 0.000000000000000000, 0.000000000000000000 ) ) ;
#2302 = EDGE_LOOP ( 'NONE', ( #7340, #5160, #6963, #458 ) ) ;
#2303 = CARTESIAN_POINT ( 'NONE',  ( 189.5040654437683258, -3.000000000000000888, 19.50000000000000711 ) ) ;
#2304 = DIRECTION ( 'NONE',  ( 1.000000000000000000, 0.000000000000000000, 0.000000000000000000 ) ) ;
#2305 = DIRECTION ( 'NONE',  ( 0.000000000000000000, 1.000000000000000000, -1.617781153285278938E-32 ) ) ;
#2306 = CARTESIAN_POINT ( 'NONE',  ( 186.9059892324150383, 5.031373033403108153, 15.00000000000000888 ) ) ;
#2307 = ADVANCED_FACE ( 'NONE', ( #1519, #2647, #989 ), #1450, .F. ) ;
#2308 = DIRECTION ( 'NONE',  ( -7.006492321624086910E-46, 1.221245327087672392E-15, -1.000000000000000000 ) ) ;
#2309 = CIRCLE ( 'NONE', #579, 3.000000000000001332 ) ;
#2310 = EDGE_LOOP ( 'NONE', ( #2244, #6766, #4084, #7389 ) ) ;
#2311 = ORIENTED_EDGE ( 'NONE', *, *, #3252, .T. ) ;
#2312 = CARTESIAN_POINT ( 'NONE',  ( 21.50000000000000000, -49.37258300203045280, -6.000000000000027534 ) ) ;
#2313 = CARTESIAN_POINT ( 'NONE',  ( 220.0000000000000000, -9.000000000000001776, 15.00000000000000888 ) ) ;
#2314 = EDGE_CURVE ( 'NONE', #4517, #2475, #871, .T. ) ;
#2315 = EDGE_LOOP ( 'NONE', ( #190, #1461 ) ) ;
#2316 = DIRECTION ( 'NONE',  ( 5.551115123125783935E-17, -0.7071067811865469066, -0.7071067811865481278 ) ) ;
#2317 = EDGE_LOOP ( 'NONE', ( #2333, #6998, #2780, #2558 ) ) ;
#2318 = PRODUCT_DEFINITION_SHAPE ( 'NONE', 'NONE',  #7608 ) ;
#2319 = CARTESIAN_POINT ( 'NONE',  ( -32.50000000000002842, 6.938893903907228378E-15, 0.000000000000000000 ) ) ;
#2320 = CARTESIAN_POINT ( 'NONE',  ( 10.25562355766779277, -218.1519544391846921, 95.22527181742790958 ) ) ;
#2321 = ORIENTED_EDGE ( 'NONE', *, *, #3305, .F. ) ;
#2322 = SHAPE_DEFINITION_REPRESENTATION ( #7500, #1206 ) ;
#2323 = CARTESIAN_POINT ( 'NONE',  ( -26.49999999999998934, -214.0630240738404666, 94.50428307177961074 ) ) ;
#2324 = DIRECTION ( 'NONE',  ( 0.000000000000000000, 0.000000000000000000, -1.000000000000000000 ) ) ;
#2325 = ORIENTED_EDGE ( 'NONE', *, *, #7457, .F. ) ;
#2326 = DIRECTION ( 'NONE',  ( 0.000000000000000000, 0.000000000000000000, -1.000000000000000000 ) ) ;
#2327 = DIRECTION ( 'NONE',  ( 5.605193857299270773E-45, 0.000000000000000000, 1.000000000000000000 ) ) ;
#2328 = DIRECTION ( 'NONE',  ( -0.7071067811865497932, -1.855836275012473479E-30, 0.7071067811865452413 ) ) ;
#2329 = DIRECTION ( 'NONE',  ( 0.000000000000000000, 0.000000000000000000, 1.000000000000000000 ) ) ;
#2330 = FACE_OUTER_BOUND ( 'NONE', #3816, .T. ) ;
#2331 = CARTESIAN_POINT ( 'NONE',  ( 217.0000000000000000, -56.99999999999999289, 7.000000000000000888 ) ) ;
#2332 = EDGE_CURVE ( 'NONE', #316, #1151, #1923, .T. ) ;
#2333 = ORIENTED_EDGE ( 'NONE', *, *, #2526, .T. ) ;
#2334 = VECTOR ( 'NONE', #3683, 1000.000000000000000 ) ;
#2335 = DIRECTION ( 'NONE',  ( 3.081487911019577365E-33, 1.193489751472043281E-15, -1.000000000000000000 ) ) ;
#2336 = DIRECTION ( 'NONE',  ( -0.000000000000000000, 1.000000000000000000, -0.000000000000000000 ) ) ;
#2337 = CARTESIAN_POINT ( 'NONE',  ( 0.000000000000000000, 0.000000000000000000, -6.999999999999992006 ) ) ;
#2338 = DIRECTION ( 'NONE',  ( 0.000000000000000000, 0.000000000000000000, -1.000000000000000000 ) ) ;
#2339 = DIRECTION ( 'NONE',  ( -1.853902270198407065E-44, -1.000000000000000000, 3.117444485084782485E-88 ) ) ;
#2340 = AXIS2_PLACEMENT_3D ( 'NONE', #634, #2866, #7558 ) ;
#2341 = ADVANCED_FACE ( 'NONE', ( #5614 ), #952, .T. ) ;
#2342 = EDGE_LOOP ( 'NONE', ( #2805, #3556, #6035, #2191 ) ) ;
#2343 = ORIENTED_EDGE ( 'NONE', *, *, #4772, .F. ) ;
#2344 = ADVANCED_BREP_SHAPE_REPRESENTATION ( '', ( #6308, #1914 ), #6340 ) ;
#2345 = CARTESIAN_POINT ( 'NONE',  ( 21.50000000000000000, 0.000000000000000000, 0.000000000000000000 ) ) ;
#2346 = CARTESIAN_POINT ( 'NONE',  ( -32.50000000000002842, 0.000000000000000000, -15.99999999999998579 ) ) ;
#2347 = VERTEX_POINT ( 'NONE', #374 ) ;
#2348 = CARTESIAN_POINT ( 'NONE',  ( -13.35769912250762559, -110.3978942797115508, 38.39789427971171420 ) ) ;
#2349 = DIRECTION ( 'NONE',  ( 7.663350976776343357E-46, 0.000000000000000000, -1.000000000000000000 ) ) ;
#2350 = AXIS2_PLACEMENT_3D ( 'NONE', #3057, #5401, #6480 ) ;
#2351 = ORIENTED_EDGE ( 'NONE', *, *, #5745, .F. ) ;
#2352 = ADVANCED_FACE ( 'NONE', ( #4539 ), #2717, .F. ) ;
#2353 = EDGE_CURVE ( 'NONE', #6501, #2614, #3225, .T. ) ;
#2354 = ORIENTED_EDGE ( 'NONE', *, *, #6948, .T. ) ;
#2355 = DIRECTION ( 'NONE',  ( -0.000000000000000000, -0.000000000000000000, 1.000000000000000000 ) ) ;
#2356 = CARTESIAN_POINT ( 'NONE',  ( 27.25616595088856542, -213.3481074634626680, 88.53882300612518463 ) ) ;
#2357 = ORIENTED_EDGE ( 'NONE', *, *, #7385, .T. ) ;
#2358 = APPLICATION_PROTOCOL_DEFINITION ( 'draft international standard', 'automotive_design', 1998, #204 ) ;
#2359 = FACE_OUTER_BOUND ( 'NONE', #4811, .T. ) ;
#2360 = DIRECTION ( 'NONE',  ( 1.000000000000000000, 0.000000000000000000, 0.000000000000000000 ) ) ;
#2361 = AXIS2_PLACEMENT_3D ( 'NONE', #5339, #72, #751 ) ;
#2362 = ORIENTED_EDGE ( 'NONE', *, *, #2533, .F. ) ;
#2363 = EDGE_CURVE ( 'NONE', #1895, #3265, #6760, .T. ) ;
#2364 = DIRECTION ( 'NONE',  ( -0.000000000000000000, 0.000000000000000000, 1.000000000000000000 ) ) ;
#2365 = VECTOR ( 'NONE', #916, 1000.000000000000114 ) ;
#2366 = LINE ( 'NONE', #2442, #1648 ) ;
#2367 = CARTESIAN_POINT ( 'NONE',  ( 47.00000000000000000, 30.03170604878415162, 10.00000000000001243 ) ) ;
#2368 = FACE_OUTER_BOUND ( 'NONE', #154, .T. ) ;
#2369 = CARTESIAN_POINT ( 'NONE',  ( 19.22480372278612037, -223.0630240738405234, 91.70218713096633678 ) ) ;
#2370 = CARTESIAN_POINT ( 'NONE',  ( 50.29734716306172970, 18.29734716306171194, 10.98910980934741310 ) ) ;
#2371 = EDGE_LOOP ( 'NONE', ( #3580, #1196, #6171, #5089 ) ) ;
#2372 = LINE ( 'NONE', #3609, #7459 ) ;
#2373 = CARTESIAN_POINT ( 'NONE',  ( -29.35769912250765046, -110.6367035073516831, 38.63670350735182524 ) ) ;
#2374 = DIRECTION ( 'NONE',  ( -3.379803290564628095E-16, -1.221245327087672392E-15, 1.000000000000000000 ) ) ;
#2375 = ADVANCED_FACE ( 'NONE', ( #2035 ), #1483, .T. ) ;
#2376 = CARTESIAN_POINT ( 'NONE',  ( 36.00000000000000000, 0.000000000000000000, 1.387778780781445676E-14 ) ) ;
#2377 = LINE ( 'NONE', #7074, #370 ) ;
#2378 = ORIENTED_EDGE ( 'NONE', *, *, #2120, .T. ) ;
#2379 = EDGE_LOOP ( 'NONE', ( #6438, #895, #6327, #5822 ) ) ;
#2380 = CARTESIAN_POINT ( 'NONE',  ( -64.50000000000000000, 0.000000000000000000, 6.000000000000000000 ) ) ;
#2381 = AXIS2_PLACEMENT_3D ( 'NONE', #542, #4018, #1003 ) ;
#2382 = DIRECTION ( 'NONE',  ( 1.000000000000000000, 0.000000000000000000, 0.000000000000000000 ) ) ;
#2383 = AXIS2_PLACEMENT_3D ( 'NONE', #1218, #5420, #1138 ) ;
#2384 = VERTEX_POINT ( 'NONE', #3807 ) ;
#2385 = CARTESIAN_POINT ( 'NONE',  ( -16.49999999999996447, -60.68629150101523351, -11.31370849898472031 ) ) ;
#2386 = CARTESIAN_POINT ( 'NONE',  ( 209.9999999999999716, -6.000000000000000000, 35.00000000000000000 ) ) ;
#2387 = LINE ( 'NONE', #7578, #308 ) ;
#2388 = VERTEX_POINT ( 'NONE', #4456 ) ;
#2389 = CIRCLE ( 'NONE', #6447, 8.500000000000007105 ) ;
#2390 = EDGE_LOOP ( 'NONE', ( #3341, #2254, #6217, #261 ) ) ;
#2391 = CARTESIAN_POINT ( 'NONE',  ( 50.00000000000000000, 21.91628335801839356, 36.91742634044857141 ) ) ;
#2392 = CARTESIAN_POINT ( 'NONE',  ( 10.21539232130207964, -217.2436419687049067, 95.06511182196837240 ) ) ;
#2393 = EDGE_LOOP ( 'NONE', ( #1733, #1705, #3392, #269 ) ) ;
#2394 = ITEM_DEFINED_TRANSFORMATION ( 'NONE', 'NONE', #4626,  #1914 ) ;
#2395 = AXIS2_PLACEMENT_3D ( 'NONE', #3388, #5732, #7455 ) ;
#2396 = CIRCLE ( 'NONE', #2149, 8.000000000000003553 ) ;
#2397 = ADVANCED_FACE ( 'NONE', ( #3846 ), #409, .T. ) ;
#2398 = DIRECTION ( 'NONE',  ( 0.000000000000000000, 0.000000000000000000, 1.000000000000000000 ) ) ;
#2399 = AXIS2_PLACEMENT_3D ( 'NONE', #6497, #6420, #5877 ) ;
#2400 = FACE_OUTER_BOUND ( 'NONE', #5121, .T. ) ;
#2401 = ORIENTED_EDGE ( 'NONE', *, *, #2272, .F. ) ;
#2402 = VECTOR ( 'NONE', #2081, 1000.000000000000000 ) ;
#2403 = LINE ( 'NONE', #4762, #6111 ) ;
#2404 = CARTESIAN_POINT ( 'NONE',  ( 25.00000000000002132, 73.78679656440357348, 0.9999999999999991118 ) ) ;
#2405 = EDGE_CURVE ( 'NONE', #1231, #2163, #5116, .T. ) ;
#2406 = LINE ( 'NONE', #7137, #618 ) ;
#2407 = PLANE ( 'NONE',  #6261 ) ;
#2408 = CIRCLE ( 'NONE', #4809, 15.99999999999997335 ) ;
#2409 = PRODUCT_DEFINITION_CONTEXT ( 'detailed design', #7413, 'design' ) ;
#2410 = ORIENTED_EDGE ( 'NONE', *, *, #4035, .T. ) ;
#2411 = AXIS2_PLACEMENT_3D ( 'NONE', #5647, #338, #2756 ) ;
#2412 = CARTESIAN_POINT ( 'NONE',  ( 188.0000000000000000, 11.00000000000000533, -7.000000000000014211 ) ) ;
#2413 = CARTESIAN_POINT ( 'NONE',  ( 3.469446951953614189E-14, 80.85786437626907741, 8.071067811865438202 ) ) ;
#2414 = CARTESIAN_POINT ( 'NONE',  ( 220.0000000000000000, 60.00000000000000000, 2.204364238465235507E-14 ) ) ;
#2415 = CARTESIAN_POINT ( 'NONE',  ( 3.000000000000000000, 56.99999999999999289, 7.000000000000022204 ) ) ;
#2416 = DIRECTION ( 'NONE',  ( 0.000000000000000000, 0.000000000000000000, 1.000000000000000000 ) ) ;
#2417 = CIRCLE ( 'NONE', #5009, 8.500000000000007105 ) ;
#2418 = ORIENTED_EDGE ( 'NONE', *, *, #772, .T. ) ;
#2419 = ADVANCED_FACE ( 'NONE', ( #3921 ), #7452, .T. ) ;
#2420 = ORIENTED_EDGE ( 'NONE', *, *, #336, .F. ) ;
#2421 = CARTESIAN_POINT ( 'NONE',  ( -13.35769912250762914, -65.39789427971170710, 38.39789427971182789 ) ) ;
#2422 = AXIS2_PLACEMENT_3D ( 'NONE', #6996, #2957, #5884 ) ;
#2423 = CARTESIAN_POINT ( 'NONE',  ( -53.43756829269515407, -222.2597742987333334, 95.94959129055638414 ) ) ;
#2424 = ORIENTED_EDGE ( 'NONE', *, *, #7381, .T. ) ;
#2425 = CARTESIAN_POINT ( 'NONE',  ( -53.43756829269602804, -227.0484711946323841, 74.34917548081359939 ) ) ;
#2426 = DIRECTION ( 'NONE',  ( -1.000000000000000000, -2.624548829666596736E-30, 9.231085635203017994E-31 ) ) ;
#2427 = FACE_OUTER_BOUND ( 'NONE', #2390, .T. ) ;
#2428 = ORIENTED_EDGE ( 'NONE', *, *, #2677, .T. ) ;
#2429 = CIRCLE ( 'NONE', #2058, 4.999999999999999112 ) ;
#2430 = EDGE_CURVE ( 'NONE', #6696, #4453, #3650, .T. ) ;
#2431 = EDGE_LOOP ( 'NONE', ( #4654, #4691 ) ) ;
#2432 = PLANE ( 'NONE',  #1390 ) ;
#2433 = CARTESIAN_POINT ( 'NONE',  ( 17.67236366837565953, -217.7372475398859137, 71.85424062197721184 ) ) ;
#2434 = EDGE_LOOP ( 'NONE', ( #274, #5135, #5652, #2679 ) ) ;
#2435 = APPLICATION_PROTOCOL_DEFINITION ( 'draft international standard', 'automotive_design', 1998, #6922 ) ;
#2436 = CYLINDRICAL_SURFACE ( 'NONE', #7018, 6.000000000000015987 ) ;
#2437 = LINE ( 'NONE', #1240, #4343 ) ;
#2438 = ORIENTED_EDGE ( 'NONE', *, *, #5232, .F. ) ;
#2439 = EDGE_CURVE ( 'NONE', #6206, #5322, #4879, .T. ) ;
#2440 = EDGE_CURVE ( 'NONE', #1259, #5789, #2776, .T. ) ;
#2441 = CARTESIAN_POINT ( 'NONE',  ( 25.00000000000000711, 28.00000000000002487, 9.999999999999996447 ) ) ;
#2442 = CARTESIAN_POINT ( 'NONE',  ( -26.50000000000000355, 16.00000000000004263, 44.76505905230376925 ) ) ;
#2443 = DIRECTION ( 'NONE',  ( -0.000000000000000000, -1.000000000000000000, -0.000000000000000000 ) ) ;
#2444 = CARTESIAN_POINT ( 'NONE',  ( 35.00000000000000000, -39.99999999999999289, 0.000000000000000000 ) ) ;
#2445 = FACE_OUTER_BOUND ( 'NONE', #3167, .T. ) ;
#2446 =( BOUNDED_CURVE ( )  B_SPLINE_CURVE ( 3, ( #1207, #3563, #4684, #2367 ),
 .UNSPECIFIED., .F., .T. ) 
 B_SPLINE_CURVE_WITH_KNOTS ( ( 4, 4 ),
 ( 4.712388980384689674, 6.283185307179586232 ),
 .UNSPECIFIED. ) 
 CURVE ( )  GEOMETRIC_REPRESENTATION_ITEM ( )  RATIONAL_B_SPLINE_CURVE ( ( 1.000000000000000000, 0.8047378541243649375, 0.8047378541243649375, 1.000000000000000000 ) ) 
 REPRESENTATION_ITEM ( '' )  );
#2447 = EDGE_CURVE ( 'NONE', #3833, #7358, #4635, .T. ) ;
#2448 = EDGE_CURVE ( 'NONE', #441, #2599, #3274, .T. ) ;
#2449 = DIRECTION ( 'NONE',  ( -0.000000000000000000, 1.000000000000000000, 0.000000000000000000 ) ) ;
#2450 = FACE_OUTER_BOUND ( 'NONE', #3737, .T. ) ;
#2451 = CARTESIAN_POINT ( 'NONE',  ( 220.0000000000000000, -56.99999999999999289, 5.510910596163094486E-16 ) ) ;
#2452 = DIRECTION ( 'NONE',  ( 1.000000000000000000, 0.000000000000000000, 0.000000000000000000 ) ) ;
#2453 = FACE_OUTER_BOUND ( 'NONE', #3471, .T. ) ;
#2454 = APPLICATION_CONTEXT ( 'automotive_design' ) ;
#2455 = ORIENTED_EDGE ( 'NONE', *, *, #1457, .F. ) ;
#2456 = EDGE_LOOP ( 'NONE', ( #5529, #3223, #950, #1622 ) ) ;
#2457 = DIRECTION ( 'NONE',  ( -1.000000000000000000, 5.551115123125783935E-17, -4.237045877651919561E-33 ) ) ;
#2458 = DIRECTION ( 'NONE',  ( -1.000000000000000000, 0.000000000000000000, -7.663350976776343357E-46 ) ) ;
#2459 = AXIS2_PLACEMENT_3D ( 'NONE', #6528, #5987, #712 ) ;
#2460 = CARTESIAN_POINT ( 'NONE',  ( -70.19709702122540307, -216.0025558445558431, 89.06679694989070128 ) ) ;
#2461 = DIRECTION ( 'NONE',  ( 2.119463927291285073E-44, 0.9997091000803153271, 0.02411877311568873250 ) ) ;
#2462 = CARTESIAN_POINT ( 'NONE',  ( -60.16175026646936885, -218.0625557288923062, 92.79915306242389761 ) ) ;
#2463 = EDGE_LOOP ( 'NONE', ( #344, #4044, #6465, #3676 ) ) ;
#2464 = VERTEX_POINT ( 'NONE', #6990 ) ;
#2465 = CARTESIAN_POINT ( 'NONE',  ( 170.0000000000000000, 11.00000000000000711, 8.660254037844383745 ) ) ;
#2466 = CARTESIAN_POINT ( 'NONE',  ( 17.77671317003690632, -224.6695236240147722, 73.71173840043843484 ) ) ;
#2467 = EDGE_LOOP ( 'NONE', ( #6362, #1439, #769, #685 ) ) ;
#2468 = EDGE_CURVE ( 'NONE', #647, #7571, #2226, .T. ) ;
#2469 = CIRCLE ( 'NONE', #1117, 10.00000000000001954 ) ;
#2470 = LINE ( 'NONE', #1276, #4813 ) ;
#2471 = FACE_OUTER_BOUND ( 'NONE', #6515, .T. ) ;
#2472 = ORIENTED_EDGE ( 'NONE', *, *, #4885, .F. ) ;
#2473 = CARTESIAN_POINT ( 'NONE',  ( 24.99999999999999289, 86.00000000000001421, 9.999999999999992895 ) ) ;
#2474 = CARTESIAN_POINT ( 'NONE',  ( 18.50000000000001421, 12.50000000000001066, 4.999999999999995559 ) ) ;
#2475 = VERTEX_POINT ( 'NONE', #2373 ) ;
#2476 =( LENGTH_UNIT ( ) NAMED_UNIT ( * ) SI_UNIT ( .MILLI., .METRE. ) );
#2477 = ADVANCED_FACE ( 'NONE', ( #4616 ), #4073, .F. ) ;
#2478 = DIRECTION ( 'NONE',  ( 0.000000000000000000, 0.9961946980917452121, 0.08715574274766277330 ) ) ;
#2479 = CARTESIAN_POINT ( 'NONE',  ( -32.50000000000002132, -59.26953873475993362, 32.26953873476001888 ) ) ;
#2480 = DIRECTION ( 'NONE',  ( 1.000000000000000000, 2.465190328815661892E-32, -9.244463733058732095E-33 ) ) ;
#2481 = UNCERTAINTY_MEASURE_WITH_UNIT (LENGTH_MEASURE( 1.000000000000000082E-05 ), #2476, 'distance_accuracy_value', 'NONE');
#2482 = VECTOR ( 'NONE', #7377, 999.9999999999998863 ) ;
#2483 = FACE_OUTER_BOUND ( 'NONE', #6804, .T. ) ;
#2484 = DIRECTION ( 'NONE',  ( 5.551115123125790098E-17, 1.000000000000000000, -8.890457814381140303E-16 ) ) ;
#2485 = FACE_OUTER_BOUND ( 'NONE', #4465, .T. ) ;
#2486 = FACE_OUTER_BOUND ( 'NONE', #2896, .T. ) ;
#2487 = CARTESIAN_POINT ( 'NONE',  ( -60.62854973486462029, -223.0631873914031473, 76.11203873288630462 ) ) ;
#2488 = CARTESIAN_POINT ( 'NONE',  ( 187.4824809480043086, -6.616222357109937668, 15.99851294154436943 ) ) ;
#2489 = ADVANCED_FACE ( 'NONE', ( #4731 ), #2911, .F. ) ;
#2490 =( BOUNDED_CURVE ( )  B_SPLINE_CURVE ( 3, ( #142, #2942, #19, #1211 ),
 .UNSPECIFIED., .F., .T. ) 
 B_SPLINE_CURVE_WITH_KNOTS ( ( 4, 4 ),
 ( 4.712388980384686121, 5.497787143782135288 ),
 .UNSPECIFIED. ) 
 CURVE ( )  GEOMETRIC_REPRESENTATION_ITEM ( )  RATIONAL_B_SPLINE_CURVE ( ( 1.000000000000000000, 0.9492530216741910110, 0.9492530216741910110, 1.000000000000000000 ) ) 
 REPRESENTATION_ITEM ( '' )  );
#2491 = EDGE_LOOP ( 'NONE', ( #3567, #4269 ) ) ;
#2492 = ORIENTED_EDGE ( 'NONE', *, *, #271, .F. ) ;
#2493 = DIRECTION ( 'NONE',  ( 0.000000000000000000, 0.000000000000000000, 1.000000000000000000 ) ) ;
#2494 = CARTESIAN_POINT ( 'NONE',  ( 21.50000000000000000, -45.34314575050758123, 18.34314575050765939 ) ) ;
#2495 = CARTESIAN_POINT ( 'NONE',  ( -53.51728042240002026, -228.8136496942592828, 74.82215363428539945 ) ) ;
#2496 = AXIS2_PLACEMENT_3D ( 'NONE', #588, #1783, #6481 ) ;
#2497 = CARTESIAN_POINT ( 'NONE',  ( 50.02171387886521359, -28.02758090397744439, 10.00000000000000533 ) ) ;
#2498 = ADVANCED_FACE ( 'NONE', ( #4109 ), #7069, .T. ) ;
#2499 = CARTESIAN_POINT ( 'NONE',  ( 217.0000000000000000, 3.000000000000000000, 35.00000000000000000 ) ) ;
#2500 = ADVANCED_FACE ( 'NONE', ( #524, #1800, #6914 ), #1636, .F. ) ;
#2501 = ORIENTED_EDGE ( 'NONE', *, *, #561, .T. ) ;
#2502 = VERTEX_POINT ( 'NONE', #1065 ) ;
#2503 = CIRCLE ( 'NONE', #5328, 8.000000000000007105 ) ;
#2504 = DIRECTION ( 'NONE',  ( -3.503246160812042677E-46, -0.7071067811865485719, -0.7071067811865464625 ) ) ;
#2505 = CARTESIAN_POINT ( 'NONE',  ( 27.12317295347672541, -221.7587214059826692, 78.74778750054862542 ) ) ;
#2506 = EDGE_LOOP ( 'NONE', ( #3320, #3127, #6602, #1126 ) ) ;
#2507 = CONTEXT_DEPENDENT_SHAPE_REPRESENTATION ( #5208, #7416 ) ;
#2508 = FACE_OUTER_BOUND ( 'NONE', #4004, .T. ) ;
#2509 = CARTESIAN_POINT ( 'NONE',  ( -32.50000000000002132, -104.2695387347598199, 32.26953873475996204 ) ) ;
#2510 = AXIS2_PLACEMENT_3D ( 'NONE', #6706, #886, #388 ) ;
#2511 = VECTOR ( 'NONE', #2225, 1000.000000000000000 ) ;
#2512 = AXIS2_PLACEMENT_3D ( 'NONE', #6237, #5704, #4553 ) ;
#2513 = EDGE_LOOP ( 'NONE', ( #5918, #1184, #4386 ) ) ;
#2514 = ADVANCED_FACE ( 'NONE', ( #2872, #5226 ), #7563, .F. ) ;
#2515 = EDGE_CURVE ( 'NONE', #2601, #722, #5843, .T. ) ;
#2516 = FACE_OUTER_BOUND ( 'NONE', #3903, .T. ) ;
#2517 = AXIS2_PLACEMENT_3D ( 'NONE', #6904, #3986, #4565 ) ;
#2518 = LINE ( 'NONE', #3062, #7428 ) ;
#2519 = CIRCLE ( 'NONE', #3501, 14.00000000000000533 ) ;
#2520 = SHAPE_REPRESENTATION_RELATIONSHIP ( 'NONE' , 'NONE' ,  #2538, #1601 ) ;
#2521 = DIRECTION ( 'NONE',  ( -1.000000000000000000, -0.000000000000000000, -0.000000000000000000 ) ) ;
#2522 = DIRECTION ( 'NONE',  ( 1.000000000000000000, 0.000000000000000000, 0.000000000000000000 ) ) ;
#2523 = LINE ( 'NONE', #1470, #2334 ) ;
#2524 = AXIS2_PLACEMENT_3D ( 'NONE', #6431, #2349, #7041 ) ;
#2525 = VECTOR ( 'NONE', #5994, 1000.000000000000000 ) ;
#2526 = EDGE_CURVE ( 'NONE', #4244, #5696, #1367, .T. ) ;
#2527 = CARTESIAN_POINT ( 'NONE',  ( 217.0000000000000000, -15.08392021690038121, 12.00000000000000711 ) ) ;
#2528 = DIRECTION ( 'NONE',  ( 0.6444004775717536715, -0.5407162030609466985, 0.5407162030609483638 ) ) ;
#2529 = DIRECTION ( 'NONE',  ( 0.000000000000000000, 0.000000000000000000, 1.000000000000000000 ) ) ;
#2530 = CARTESIAN_POINT ( 'NONE',  ( -64.49542967829545148, -223.0630240738403813, 84.38699617518491891 ) ) ;
#2531 = DIRECTION ( 'NONE',  ( 0.000000000000000000, 0.000000000000000000, 1.000000000000000000 ) ) ;
#2532 = EDGE_LOOP ( 'NONE', ( #6594, #4006 ) ) ;
#2533 = EDGE_CURVE ( 'NONE', #2116, #2534, #642, .T. ) ;
#2534 = VERTEX_POINT ( 'NONE', #4842 ) ;
#2535 = ADVANCED_FACE ( 'NONE', ( #6641 ), #4225, .F. ) ;
#2536 = DIRECTION ( 'NONE',  ( 1.000000000000000000, 0.000000000000000000, 0.000000000000000000 ) ) ;
#2537 = DIRECTION ( 'NONE',  ( 1.000000000000000000, 0.000000000000000000, 0.000000000000000000 ) ) ;
#2538 = SHAPE_REPRESENTATION ( 'large revit', ( #1914 ), #5969 ) ;
#2539 = DIRECTION ( 'NONE',  ( -2.465190328815662439E-32, -1.000000000000000000, 0.000000000000000000 ) ) ;
#2540 = VECTOR ( 'NONE', #6220, 1000.000000000000114 ) ;
#2541 = DIRECTION ( 'NONE',  ( 1.000000000000000000, 2.465190328815661892E-32, -9.244463733058732095E-33 ) ) ;
#2542 = CARTESIAN_POINT ( 'NONE',  ( -60.75147712453755844, -218.0628479320674842, 92.28982506784103634 ) ) ;
#2543 = ORIENTED_EDGE ( 'NONE', *, *, #7307, .T. ) ;
#2544 = ORIENTED_EDGE ( 'NONE', *, *, #603, .F. ) ;
#2545 = ADVANCED_FACE ( 'NONE', ( #4263 ), #2988, .F. ) ;
#2546 = DIRECTION ( 'NONE',  ( -0.000000000000000000, 0.03489949670250429292, 0.9993908270190955401 ) ) ;
#2547 = CARTESIAN_POINT ( 'NONE',  ( 10.33013951010423170, -224.6695236240153122, 73.71173840043077519 ) ) ;
#2548 = ORIENTED_EDGE ( 'NONE', *, *, #4878, .F. ) ;
#2549 = FACE_OUTER_BOUND ( 'NONE', #5959, .T. ) ;
#2550 = DIRECTION ( 'NONE',  ( -1.000000000000000000, 5.551115123125783935E-17, -4.237045877651919561E-33 ) ) ;
#2551 = AXIS2_PLACEMENT_3D ( 'NONE', #4323, #3168, #6665 ) ;
#2552 = ORIENTED_EDGE ( 'NONE', *, *, #3301, .T. ) ;
#2553 = DIRECTION ( 'NONE',  ( -1.000000000000000000, -2.624548829666596736E-30, 9.231085635203017994E-31 ) ) ;
#2554 = DIRECTION ( 'NONE',  ( -5.605193857299270773E-45, -0.000000000000000000, -1.000000000000000000 ) ) ;
#2555 = APPLICATION_CONTEXT ( 'automotive_design' ) ;
#2556 = LINE ( 'NONE', #3098, #4823 ) ;
#2557 = CARTESIAN_POINT ( 'NONE',  ( -27.00000000000000000, 3.306546357697852550E-15, -6.999999999999992006 ) ) ;
#2558 = ORIENTED_EDGE ( 'NONE', *, *, #6113, .F. ) ;
#2559 = CARTESIAN_POINT ( 'NONE',  ( 0.000000000000000000, 0.000000000000000000, 0.000000000000000000 ) ) ;
#2560 = FILL_AREA_STYLE ('',( #2637 ) ) ;
#2561 = CARTESIAN_POINT ( 'NONE',  ( 25.00000000000001421, 35.07106781186547551, 2.928932188134525827 ) ) ;
#2562 = CARTESIAN_POINT ( 'NONE',  ( -63.95077716541958068, -223.0623318094975502, 88.33193110890873356 ) ) ;
#2563 = ORIENTED_EDGE ( 'NONE', *, *, #4005, .F. ) ;
#2564 = DIRECTION ( 'NONE',  ( 0.000000000000000000, 0.000000000000000000, -1.000000000000000000 ) ) ;
#2565 = ADVANCED_FACE ( 'NONE', ( #3725 ), #1872, .T. ) ;
#2566 = EDGE_LOOP ( 'NONE', ( #5546, #4779, #538, #7197 ) ) ;
#2567 = ORIENTED_EDGE ( 'NONE', *, *, #5163, .T. ) ;
#2568 = DIRECTION ( 'NONE',  ( 1.000000000000000000, 2.465190328815661892E-32, -9.244463733058732095E-33 ) ) ;
#2569 = CARTESIAN_POINT ( 'NONE',  ( 217.0000000000000000, 9.000000000000001776, 18.00000000000001066 ) ) ;
#2570 = DIRECTION ( 'NONE',  ( 0.000000000000000000, 0.03489949670250429292, 0.9993908270190955401 ) ) ;
#2571 = EDGE_CURVE ( 'NONE', #5363, #6577, #5306, .T. ) ;
#2572 = CARTESIAN_POINT ( 'NONE',  ( 186.9059892324150383, 6.000000000000000000, 18.00000000000001066 ) ) ;
#2573 = CARTESIAN_POINT ( 'NONE',  ( -62.21889548225904321, -218.0624042392298634, 90.69967475268330759 ) ) ;
#2574 = VERTEX_POINT ( 'NONE', #4915 ) ;
#2575 = VERTEX_POINT ( 'NONE', #1982 ) ;
#2576 = LINE ( 'NONE', #1423, #4970 ) ;
#2577 = FACE_OUTER_BOUND ( 'NONE', #13, .T. ) ;
#2578 = VERTEX_POINT ( 'NONE', #3687 ) ;
#2579 = DIRECTION ( 'NONE',  ( 0.6427876096865583477, 9.159339953157543431E-16, -0.7660444431189621373 ) ) ;
#2580 = CARTESIAN_POINT ( 'NONE',  ( 170.0000000000000000, 0.000000000000000000, 0.000000000000000000 ) ) ;
#2581 = ADVANCED_FACE ( 'NONE', ( #4336 ), #1402, .F. ) ;
#2582 = AXIS2_PLACEMENT_3D ( 'NONE', #5030, #3728, #226 ) ;
#2583 = VERTEX_POINT ( 'NONE', #2413 ) ;
#2584 = DIRECTION ( 'NONE',  ( -1.000000000000000000, 0.000000000000000000, -7.663350976776343357E-46 ) ) ;
#2585 = AXIS2_PLACEMENT_3D ( 'NONE', #5449, #7214, #1468 ) ;
#2586 = CARTESIAN_POINT ( 'NONE',  ( -10.49999999999996803, 0.000000000000000000, 0.000000000000000000 ) ) ;
#2587 = ORIENTED_EDGE ( 'NONE', *, *, #5314, .T. ) ;
#2588 = DIRECTION ( 'NONE',  ( 1.000000000000000000, 0.000000000000000000, 0.000000000000000000 ) ) ;
#2589 = DIRECTION ( 'NONE',  ( 0.000000000000000000, -8.673617379884050263E-16, -1.000000000000000000 ) ) ;
#2590 = DIRECTION ( 'NONE',  ( -1.000000000000000000, 0.000000000000000000, -7.663350976776343357E-46 ) ) ;
#2591 = ADVANCED_FACE ( 'NONE', ( #1255 ), #3611, .T. ) ;
#2592 = CIRCLE ( 'NONE', #5174, 15.99999999999997691 ) ;
#2593 =( REPRESENTATION_RELATIONSHIP ('NONE','NONE', #4862, #1206 ) REPRESENTATION_RELATIONSHIP_WITH_TRANSFORMATION ( #6086 )SHAPE_REPRESENTATION_RELATIONSHIP( ) );
#2594 = CARTESIAN_POINT ( 'NONE',  ( -53.25168462842736261, -218.0630240738404950, 95.20959099461346398 ) ) ;
#2595 = VECTOR ( 'NONE', #6129, 1000.000000000000000 ) ;
#2596 = CARTESIAN_POINT ( 'NONE',  ( 3.000000000000002665, -28.78532416918554304, 13.00000000000000711 ) ) ;
#2597 = CYLINDRICAL_SURFACE ( 'NONE', #4621, 15.99999999999999645 ) ;
#2598 = CARTESIAN_POINT ( 'NONE',  ( -59.74328897643390235, -223.0635515775393856, 75.39397519229926559 ) ) ;
#2599 = VERTEX_POINT ( 'NONE', #3033 ) ;
#2600 = DIRECTION ( 'NONE',  ( 1.000000000000000000, 0.000000000000000000, 0.000000000000000000 ) ) ;
#2601 = VERTEX_POINT ( 'NONE', #6029 ) ;
#2602 = EDGE_LOOP ( 'NONE', ( #3213, #6753, #4625, #1688 ) ) ;
#2603 = EDGE_CURVE ( 'NONE', #258, #1604, #1987, .T. ) ;
#2604 = CARTESIAN_POINT ( 'NONE',  ( 0.000000000000000000, 0.000000000000000000, -6.999999999999992006 ) ) ;
#2605 = EDGE_CURVE ( 'NONE', #1241, #3224, #183, .T. ) ;
#2606 = CARTESIAN_POINT ( 'NONE',  ( -64.50000000000000000, -120.9522879036833416, 45.92078884797942351 ) ) ;
#2607 = CARTESIAN_POINT ( 'NONE',  ( 23.99999999999999289, 0.000000000000000000, -6.999999999999992006 ) ) ;
#2608 = CARTESIAN_POINT ( 'NONE',  ( 26.00000000000000000, -7.873646488999802468E-30, 9.999999999999998224 ) ) ;
#2609 = ORIENTED_EDGE ( 'NONE', *, *, #1176, .T. ) ;
#2610 = ORIENTED_EDGE ( 'NONE', *, *, #6448, .F. ) ;
#2611 = TOROIDAL_SURFACE ( 'NONE', #1881, 6.000000000000000000, 3.000000000000000000 ) ;
#2612 = LINE ( 'NONE', #2652, #912 ) ;
#2613 = DIRECTION ( 'NONE',  ( 0.000000000000000000, 0.9961946980917452121, 0.08715574274766219043 ) ) ;
#2614 = VERTEX_POINT ( 'NONE', #3071 ) ;
#2615 = CONTEXT_DEPENDENT_SHAPE_REPRESENTATION ( #4182, #3489 ) ;
#2616 = CARTESIAN_POINT ( 'NONE',  ( -29.35769912250765046, 16.00000000000004263, 38.63670350735201708 ) ) ;
#2617 = DIRECTION ( 'NONE',  ( -2.465190328815661892E-32, -1.000000000000000000, -1.193489751472043281E-15 ) ) ;
#2618 = VERTEX_POINT ( 'NONE', #4529 ) ;
#2619 = AXIS2_PLACEMENT_3D ( 'NONE', #7475, #6242, #395 ) ;
#2620 = LINE ( 'NONE', #4982, #3415 ) ;
#2621 = EDGE_CURVE ( 'NONE', #4871, #3617, #4327, .T. ) ;
#2622 = CARTESIAN_POINT ( 'NONE',  ( 50.02171387886895815, 29.27153168735074829, 10.00000000000000888 ) ) ;
#2623 = LINE ( 'NONE', #4256, #4120 ) ;
#2624 = VERTEX_POINT ( 'NONE', #6750 ) ;
#2625 =( NAMED_UNIT ( * ) SI_UNIT ( $, .STERADIAN. ) SOLID_ANGLE_UNIT ( ) );
#2626 = CIRCLE ( 'NONE', #1278, 3.000000000000000000 ) ;
#2627 = DIRECTION ( 'NONE',  ( 1.000000000000000000, 0.000000000000000000, 0.000000000000000000 ) ) ;
#2628 = AXIS2_PLACEMENT_3D ( 'NONE', #4380, #5491, #2484 ) ;
#2629 = LINE ( 'NONE', #6859, #1351 ) ;
#2630 = PRESENTATION_STYLE_ASSIGNMENT (( #2016 ) ) ;
#2631 = ORIENTED_EDGE ( 'NONE', *, *, #5085, .F. ) ;
#2632 = EDGE_LOOP ( 'NONE', ( #3459, #4988, #6672, #7530 ) ) ;
#2633 = CIRCLE ( 'NONE', #3870, 6.000000000000000888 ) ;
#2634 = AXIS2_PLACEMENT_3D ( 'NONE', #4040, #1102, #5804 ) ;
#2635 = FACE_OUTER_BOUND ( 'NONE', #2371, .T. ) ;
#2636 = EDGE_CURVE ( 'NONE', #2722, #1494, #7363, .T. ) ;
#2637 = FILL_AREA_STYLE_COLOUR ( '', #6316 ) ;
#2638 = CARTESIAN_POINT ( 'NONE',  ( 21.50000000000000000, 0.000000000000000000, 0.000000000000000000 ) ) ;
#2639 = CARTESIAN_POINT ( 'NONE',  ( -64.40058489821628029, -223.0610658478785524, 86.48602887601485634 ) ) ;
#2640 = CARTESIAN_POINT ( 'NONE',  ( 186.9464243967159121, -5.771739343384286514, 15.00000000000000888 ) ) ;
#2641 = LINE ( 'NONE', #946, #2767 ) ;
#2642 = CIRCLE ( 'NONE', #6944, 2.999999999999999112 ) ;
#2643 = CIRCLE ( 'NONE', #3636, 3.000000000000000000 ) ;
#2644 = CIRCLE ( 'NONE', #4371, 2.999999999999999112 ) ;
#2645 = ORIENTED_EDGE ( 'NONE', *, *, #1927, .T. ) ;
#2646 = ORIENTED_EDGE ( 'NONE', *, *, #3787, .T. ) ;
#2647 = FACE_BOUND ( 'NONE', #6328, .T. ) ;
#2648 = DIRECTION ( 'NONE',  ( 5.605193857299270773E-45, 0.000000000000000000, 1.000000000000000000 ) ) ;
#2649 = DIRECTION ( 'NONE',  ( 0.000000000000000000, 0.000000000000000000, -1.000000000000000000 ) ) ;
#2650 = VERTEX_POINT ( 'NONE', #3837 ) ;
#2651 = ORIENTED_EDGE ( 'NONE', *, *, #2075, .T. ) ;
#2652 = CARTESIAN_POINT ( 'NONE',  ( 220.0000000000000000, 56.99999999999999289, 2.149255132503604690E-14 ) ) ;
#2653 = ORIENTED_EDGE ( 'NONE', *, *, #6027, .F. ) ;
#2654 = CARTESIAN_POINT ( 'NONE',  ( -10.49999999999996803, -49.37258300203045280, 5.999999999999972466 ) ) ;
#2655 = CARTESIAN_POINT ( 'NONE',  ( 12.50000000000000355, 101.5000000000000000, -1.214306433183764966E-14 ) ) ;
#2656 = ADVANCED_FACE ( 'NONE', ( #899 ), #6790, .F. ) ;
#2657 = ORIENTED_EDGE ( 'NONE', *, *, #3250, .T. ) ;
#2658 = AXIS2_PLACEMENT_3D ( 'NONE', #1944, #7067, #3068 ) ;
#2659 = B_SPLINE_CURVE_WITH_KNOTS ( 'NONE', 3,
 ( #2853, #6364, #6975, #1699 ),
 .UNSPECIFIED., .F., .F.,
 ( 4, 4 ),
 ( 0.000000000000000000, 1.000000000000000000 ),
 .UNSPECIFIED. ) ;
#2660 = DIRECTION ( 'NONE',  ( 1.000000000000000000, 0.000000000000000000, 0.000000000000000000 ) ) ;
#2661 = CARTESIAN_POINT ( 'NONE',  ( -13.64230087749234599, -110.6367035073516689, 38.63670350735182524 ) ) ;
#2662 = FACE_BOUND ( 'NONE', #857, .T. ) ;
#2663 = VERTEX_POINT ( 'NONE', #5636 ) ;
#2664 = CIRCLE ( 'NONE', #4159, 13.99999999999999645 ) ;
#2665 = CARTESIAN_POINT ( 'NONE',  ( -60.76462208873360282, -219.0153713307823580, 95.37751551101587211 ) ) ;
#2666 = DIRECTION ( 'NONE',  ( -7.006492321624086910E-46, 1.221245327087672392E-15, -1.000000000000000000 ) ) ;
#2667 = CARTESIAN_POINT ( 'NONE',  ( 203.9378221735088914, 3.000000000000000000, 38.49999999999998579 ) ) ;
#2668 = ADVANCED_FACE ( 'NONE', ( #360 ), #6709, .T. ) ;
#2669 = ORIENTED_EDGE ( 'NONE', *, *, #3776, .F. ) ;
#2670 = ORIENTED_EDGE ( 'NONE', *, *, #5988, .T. ) ;
#2671 = CARTESIAN_POINT ( 'NONE',  ( -26.49999999999999645, -105.5631177942458407, 67.24940929526130162 ) ) ;
#2672 = DIRECTION ( 'NONE',  ( 0.000000000000000000, 0.000000000000000000, -1.000000000000000000 ) ) ;
#2673 = CARTESIAN_POINT ( 'NONE',  ( 1.387778780781445676E-14, 12.49999999999998401, 4.999999999999999112 ) ) ;
#2674 = CARTESIAN_POINT ( 'NONE',  ( -64.50000000000000000, 0.000000000000000000, 0.000000000000000000 ) ) ;
#2675 = CARTESIAN_POINT ( 'NONE',  ( -16.50000000000001066, -216.4061698243480691, 94.91744288732648727 ) ) ;
#2676 = DIRECTION ( 'NONE',  ( -1.853902270198407313E-44, -1.000000000000000000, 0.000000000000000000 ) ) ;
#2677 = EDGE_CURVE ( 'NONE', #312, #589, #709, .T. ) ;
#2678 = EDGE_CURVE ( 'NONE', #2475, #7561, #6668, .T. ) ;
#2679 = ORIENTED_EDGE ( 'NONE', *, *, #171, .F. ) ;
#2680 = VERTEX_POINT ( 'NONE', #4835 ) ;
#2681 = PRODUCT_RELATED_PRODUCT_CATEGORY ( 'part', '', ( #3210 ) ) ;
#2682 = CARTESIAN_POINT ( 'NONE',  ( 0.000000000000000000, -28.78532416918554304, 13.00000000000000711 ) ) ;
#2683 = DIRECTION ( 'NONE',  ( 5.605193857299270773E-45, 0.000000000000000000, 1.000000000000000000 ) ) ;
#2684 = DIRECTION ( 'NONE',  ( 1.000000000000000000, 0.000000000000000000, 0.000000000000000000 ) ) ;
#2685 = LINE ( 'NONE', #3772, #6662 ) ;
#2686 = EDGE_CURVE ( 'NONE', #233, #1634, #6898, .T. ) ;
#2687 = EDGE_LOOP ( 'NONE', ( #2492, #2438, #1073, #3672 ) ) ;
#2688 = ORIENTED_EDGE ( 'NONE', *, *, #4139, .F. ) ;
#2689 = CARTESIAN_POINT ( 'NONE',  ( 36.00000000000000000, -4.163336342344337027E-14, 10.00000000000001243 ) ) ;
#2690 = ORIENTED_EDGE ( 'NONE', *, *, #1361, .T. ) ;
#2691 = CARTESIAN_POINT ( 'NONE',  ( 0.000000000000000000, 0.000000000000000000, -3.000000000000002665 ) ) ;
#2692 = CARTESIAN_POINT ( 'NONE',  ( 220.0000000000000000, -28.78532416918554304, 13.00000000000000711 ) ) ;
#2693 = APPLICATION_CONTEXT ( 'automotive_design' ) ;
#2694 = ORIENTED_EDGE ( 'NONE', *, *, #2215, .F. ) ;
#2695 = AXIS2_PLACEMENT_3D ( 'NONE', #1590, #519, #3990 ) ;
#2696 = EDGE_CURVE ( 'NONE', #459, #1421, #6775, .T. ) ;
#2697 = CARTESIAN_POINT ( 'NONE',  ( 0.000000000000000000, 0.000000000000000000, -3.000000000000002665 ) ) ;
#2698 = VERTEX_POINT ( 'NONE', #3136 ) ;
#2699 = DIRECTION ( 'NONE',  ( 1.000000000000000000, 0.000000000000000000, 0.000000000000000000 ) ) ;
#2700 = CARTESIAN_POINT ( 'NONE',  ( -53.10580595754474587, -214.7694783647500856, 94.62885002390424916 ) ) ;
#2701 = DIRECTION ( 'NONE',  ( 0.000000000000000000, 1.000000000000000000, 1.734723475976805517E-15 ) ) ;
#2702 = AXIS2_PLACEMENT_3D ( 'NONE', #7294, #5495, #1478 ) ;
#2703 = DIRECTION ( 'NONE',  ( 0.000000000000000000, 0.000000000000000000, 1.000000000000000000 ) ) ;
#2704 = ORIENTED_EDGE ( 'NONE', *, *, #2007, .T. ) ;
#2705 = ORIENTED_EDGE ( 'NONE', *, *, #7577, .T. ) ;
#2706 = AXIS2_PLACEMENT_3D ( 'NONE', #3793, #854, #507 ) ;
#2707 = DIRECTION ( 'NONE',  ( 4.622231866529368100E-33, -2.600005424922769496E-32, 1.000000000000000000 ) ) ;
#2708 = EDGE_CURVE ( 'NONE', #7449, #191, #2556, .T. ) ;
#2709 = CARTESIAN_POINT ( 'NONE',  ( 187.3640976635304298, 4.216080228656712947, 15.79346707806755745 ) ) ;
#2710 = CARTESIAN_POINT ( 'NONE',  ( -63.43106901615326620, -223.0630240738406087, 89.73152280343640541 ) ) ;
#2711 = DIRECTION ( 'NONE',  ( 0.000000000000000000, 0.000000000000000000, 1.000000000000000000 ) ) ;
#2712 = DIRECTION ( 'NONE',  ( -0.000000000000000000, 0.08715574274766212104, -0.9961946980917452121 ) ) ;
#2713 = CARTESIAN_POINT ( 'NONE',  ( -63.02662698389872986, -218.0624813771180470, 89.41762891734713037 ) ) ;
#2714 = VERTEX_POINT ( 'NONE', #215 ) ;
#2715 = EDGE_LOOP ( 'NONE', ( #3981, #4050, #326, #7035 ) ) ;
#2716 = DIRECTION ( 'NONE',  ( 8.747574602982982877E-17, -0.9659258262890683122, 0.2588190451025209060 ) ) ;
#2717 = CYLINDRICAL_SURFACE ( 'NONE', #1546, 2.999999999999999112 ) ;
#2718 = DIRECTION ( 'NONE',  ( 0.000000000000000000, 0.08715574274766212104, -0.9961946980917452121 ) ) ;
#2719 = ADVANCED_FACE ( 'NONE', ( #4406 ), #1391, .T. ) ;
#2720 = DIRECTION ( 'NONE',  ( 0.000000000000000000, 0.000000000000000000, -1.000000000000000000 ) ) ;
#2721 = ORIENTED_EDGE ( 'NONE', *, *, #4245, .F. ) ;
#2722 = VERTEX_POINT ( 'NONE', #5985 ) ;
#2723 = AXIS2_PLACEMENT_3D ( 'NONE', #5848, #2951, #4697 ) ;
#2724 = CARTESIAN_POINT ( 'NONE',  ( 173.9999999999999716, -10.95994505756729254, 7.000000000000016875 ) ) ;
#2725 = EDGE_CURVE ( 'NONE', #505, #7420, #3792, .T. ) ;
#2726 = VERTEX_POINT ( 'NONE', #3065 ) ;
#2727 = DIRECTION ( 'NONE',  ( -0.000000000000000000, -1.000000000000000000, -0.000000000000000000 ) ) ;
#2728 = DIRECTION ( 'NONE',  ( 0.000000000000000000, 1.301042606982600785E-15, -1.000000000000000000 ) ) ;
#2729 = ADVANCED_FACE ( 'NONE', ( #1323 ), #3758, .T. ) ;
#2730 = VERTEX_POINT ( 'NONE', #140 ) ;
#2731 = CARTESIAN_POINT ( 'NONE',  ( 47.78553976602684372, 30.03170604878551586, 10.00000000000000888 ) ) ;
#2732 = CARTESIAN_POINT ( 'NONE',  ( -32.50000000000002132, 16.00000000000006750, 32.26953873476009704 ) ) ;
#2733 = EDGE_LOOP ( 'NONE', ( #500, #4088, #1774, #3184 ) ) ;
#2734 = LINE ( 'NONE', #6744, #3353 ) ;
#2735 = CARTESIAN_POINT ( 'NONE',  ( 4.000000000000003553, 0.000000000000000000, 1.387778780781445676E-14 ) ) ;
#2736 = DIRECTION ( 'NONE',  ( 1.000000000000000000, 0.000000000000000000, 0.000000000000000000 ) ) ;
#2737 = ORIENTED_EDGE ( 'NONE', *, *, #3912, .F. ) ;
#2738 = ORIENTED_EDGE ( 'NONE', *, *, #5642, .T. ) ;
#2739 = EDGE_CURVE ( 'NONE', #5684, #1669, #852, .T. ) ;
#2740 = CARTESIAN_POINT ( 'NONE',  ( 201.3397459621555754, 6.000000000000000000, 39.99999999999997868 ) ) ;
#2741 = CIRCLE ( 'NONE', #3984, 13.99999999999999112 ) ;
#2742 = CIRCLE ( 'NONE', #1766, 6.000000000000001776 ) ;
#2743 =( LENGTH_UNIT ( ) NAMED_UNIT ( * ) SI_UNIT ( .MILLI., .METRE. ) );
#2744 = DIRECTION ( 'NONE',  ( -5.551115123125783935E-17, -1.000000000000000000, -5.166928274020107963E-17 ) ) ;
#2745 = DIRECTION ( 'NONE',  ( 1.000000000000000000, 0.000000000000000000, 7.663350976776343357E-46 ) ) ;
#2746 = AXIS2_PLACEMENT_3D ( 'NONE', #3480, #7050, #12 ) ;
#2747 = CARTESIAN_POINT ( 'NONE',  ( -62.25770276840173523, -223.0625327031958136, 91.64692538425377677 ) ) ;
#2748 = DIRECTION ( 'NONE',  ( 1.000000000000000000, 1.725633230170963324E-31, -1.078147950931789387E-16 ) ) ;
#2749 = CARTESIAN_POINT ( 'NONE',  ( -16.49999999999998934, -117.9145199278634522, 44.76505905230362714 ) ) ;
#2750 = CARTESIAN_POINT ( 'NONE',  ( -63.59392405224133427, -218.0630241027633360, 79.12603136341994059 ) ) ;
#2751 = AXIS2_PLACEMENT_3D ( 'NONE', #2569, #1955, #4962 ) ;
#2752 = CIRCLE ( 'NONE', #3622, 7.999999999999992895 ) ;
#2753 = ORIENTED_EDGE ( 'NONE', *, *, #4174, .F. ) ;
#2754 = ORIENTED_EDGE ( 'NONE', *, *, #3348, .T. ) ;
#2755 = CARTESIAN_POINT ( 'NONE',  ( 217.0000000000000000, -15.08392021690038121, 15.00000000000000888 ) ) ;
#2756 = DIRECTION ( 'NONE',  ( 0.000000000000000000, 0.000000000000000000, 1.000000000000000000 ) ) ;
#2757 = CIRCLE ( 'NONE', #7064, 3.000000000000002665 ) ;
#2758 = CARTESIAN_POINT ( 'NONE',  ( 35.75983027283935201, -69.18339347973481779, -2.816606520265163560 ) ) ;
#2759 = CARTESIAN_POINT ( 'NONE',  ( 217.0000000000000000, -56.99999999999999289, 7.000000000000000888 ) ) ;
#2760 = CIRCLE ( 'NONE', #5221, 7.999999999999992895 ) ;
#2761 = AXIS2_PLACEMENT_3D ( 'NONE', #1562, #3344, #990 ) ;
#2762 = CARTESIAN_POINT ( 'NONE',  ( -16.50000000000000000, -99.90626354475340065, 72.90626354475362803 ) ) ;
#2763 = ADVANCED_FACE ( 'NONE', ( #3680 ), #779, .T. ) ;
#2764 = ORIENTED_EDGE ( 'NONE', *, *, #2678, .T. ) ;
#2765 = AXIS2_PLACEMENT_3D ( 'NONE', #704, #4359, #133 ) ;
#2766 = ADVANCED_FACE ( 'NONE', ( #6097 ), #7171, .T. ) ;
#2767 = VECTOR ( 'NONE', #4492, 1000.000000000000000 ) ;
#2768 = VERTEX_POINT ( 'NONE', #4258 ) ;
#2769 = DIRECTION ( 'NONE',  ( 0.000000000000000000, 1.000000000000000000, -6.223320470066798607E-15 ) ) ;
#2770 = ORIENTED_EDGE ( 'NONE', *, *, #3884, .F. ) ;
#2771 = CARTESIAN_POINT ( 'NONE',  ( -16.49999999999997513, -104.8363803175325160, 32.83638031753267938 ) ) ;
#2772 = CARTESIAN_POINT ( 'NONE',  ( -21.51784377693468642, -113.7796841263389069, 41.77968412633906325 ) ) ;
#2773 = ORIENTED_EDGE ( 'NONE', *, *, #5931, .F. ) ;
#2774 = ADVANCED_FACE ( 'NONE', ( #6599 ), #3714, .F. ) ;
#2775 = EDGE_CURVE ( 'NONE', #5563, #2574, #7391, .T. ) ;
#2776 = CIRCLE ( 'NONE', #2171, 15.99999999999998934 ) ;
#2777 = PRODUCT_RELATED_PRODUCT_CATEGORY ( 'part', '', ( #3413 ) ) ;
#2778 = CYLINDRICAL_SURFACE ( 'NONE', #5463, 3.000000000000000000 ) ;
#2779 = CARTESIAN_POINT ( 'NONE',  ( 40.00000000000000000, -4.040871662429601878E-14, -9.999999999999984013 ) ) ;
#2780 = ORIENTED_EDGE ( 'NONE', *, *, #1317, .F. ) ;
#2781 = LINE ( 'NONE', #6783, #4711 ) ;
#2782 = LINE ( 'NONE', #4095, #4561 ) ;
#2783 =( BOUNDED_CURVE ( )  B_SPLINE_CURVE ( 3, ( #2121, #5595, #319, #7320 ),
 .UNSPECIFIED., .F., .T. ) 
 B_SPLINE_CURVE_WITH_KNOTS ( ( 4, 4 ),
 ( 1.570796326794896114, 2.418858405776376230 ),
 .UNSPECIFIED. ) 
 CURVE ( )  GEOMETRIC_REPRESENTATION_ITEM ( )  RATIONAL_B_SPLINE_CURVE ( ( 1.000000000000000000, 0.9409585518440986007, 0.9409585518440986007, 1.000000000000000000 ) ) 
 REPRESENTATION_ITEM ( '' )  );
#2784 = DIRECTION ( 'NONE',  ( 0.000000000000000000, 0.000000000000000000, -1.000000000000000000 ) ) ;
#2785 = ORIENTED_EDGE ( 'NONE', *, *, #5085, .T. ) ;
#2786 = VERTEX_POINT ( 'NONE', #2013 ) ;
#2787 = AXIS2_PLACEMENT_3D ( 'NONE', #4297, #4730, #1797 ) ;
#2788 = CARTESIAN_POINT ( 'NONE',  ( 50.00000000000000000, 17.91234734164656928, 13.00000000000000711 ) ) ;
#2789 = CARTESIAN_POINT ( 'NONE',  ( 176.5000000000000000, -39.99999999999999289, 0.000000000000000000 ) ) ;
#2790 = DIRECTION ( 'NONE',  ( 1.000000000000000000, 2.465190328815661892E-32, -9.244463733058732095E-33 ) ) ;
#2791 = CARTESIAN_POINT ( 'NONE',  ( 209.9999999999999716, 6.000000000000000000, 35.00000000000000000 ) ) ;
#2792 = CARTESIAN_POINT ( 'NONE',  ( -10.49999999999997513, -6.938893903907228378E-15, 15.99999999999998579 ) ) ;
#2793 = CARTESIAN_POINT ( 'NONE',  ( -63.78893983331448680, -218.0634842797883550, 79.62726457540794911 ) ) ;
#2794 = AXIS2_PLACEMENT_3D ( 'NONE', #2441, #6559, #5443 ) ;
#2795 = VERTEX_POINT ( 'NONE', #4520 ) ;
#2796 = VERTEX_POINT ( 'NONE', #6858 ) ;
#2797 = FACE_OUTER_BOUND ( 'NONE', #1737, .T. ) ;
#2798 = DIRECTION ( 'NONE',  ( 0.000000000000000000, 0.000000000000000000, -1.000000000000000000 ) ) ;
#2799 = CARTESIAN_POINT ( 'NONE',  ( -21.50000000000000000, -215.0630240738404950, 94.68061005248806339 ) ) ;
#2800 = EDGE_CURVE ( 'NONE', #4118, #7372, #7472, .T. ) ;
#2801 = FACE_OUTER_BOUND ( 'NONE', #4525, .T. ) ;
#2802 = EDGE_CURVE ( 'NONE', #2795, #3147, #6782, .T. ) ;
#2803 = LINE ( 'NONE', #456, #3843 ) ;
#2804 = ORIENTED_EDGE ( 'NONE', *, *, #5176, .T. ) ;
#2805 = ORIENTED_EDGE ( 'NONE', *, *, #7397, .T. ) ;
#2806 = CARTESIAN_POINT ( 'NONE',  ( 220.0000000000000000, -60.00000000000000000, 0.000000000000000000 ) ) ;
#2807 = EDGE_CURVE ( 'NONE', #3862, #5693, #2781, .T. ) ;
#2808 = PLANE ( 'NONE',  #1647 ) ;
#2809 = VERTEX_POINT ( 'NONE', #3288 ) ;
#2810 = CARTESIAN_POINT ( 'NONE',  ( -16.49999999999996447, -49.37258300203045280, -2.775557561562891351E-14 ) ) ;
#2811 = LINE ( 'NONE', #3856, #2281 ) ;
#2812 = ORIENTED_EDGE ( 'NONE', *, *, #6304, .F. ) ;
#2813 = DIRECTION ( 'NONE',  ( -0.000000000000000000, -0.000000000000000000, -1.000000000000000000 ) ) ;
#2814 = CARTESIAN_POINT ( 'NONE',  ( 27.08493024494318746, -221.0431231857559737, 90.06937369499782164 ) ) ;
#2815 = ORIENTED_EDGE ( 'NONE', *, *, #1965, .F. ) ;
#2816 = SHAPE_REPRESENTATION_RELATIONSHIP ( 'NONE' , 'NONE' ,  #1206, #4093 ) ;
#2817 = CARTESIAN_POINT ( 'NONE',  ( -53.48785751550376233, -223.3951688904016635, 96.14979199081800232 ) ) ;
#2818 = ADVANCED_FACE ( 'NONE', ( #1578 ), #5706, .F. ) ;
#2819 = CARTESIAN_POINT ( 'NONE',  ( 24.99999999999999289, 86.00000000000001421, 9.999999999999992895 ) ) ;
#2820 = CARTESIAN_POINT ( 'NONE',  ( -13.22915763683106327, -74.27084236316865429, 47.27084236316875376 ) ) ;
#2821 = VERTEX_POINT ( 'NONE', #3937 ) ;
#2822 = ORIENTED_EDGE ( 'NONE', *, *, #5881, .F. ) ;
#2823 = CARTESIAN_POINT ( 'NONE',  ( 50.04196010845020481, 18.04196010845019060, 12.50000000000000711 ) ) ;
#2824 = SURFACE_SIDE_STYLE ('',( #359 ) ) ;
#2825 = VECTOR ( 'NONE', #595, 1000.000000000000000 ) ;
#2826 = CARTESIAN_POINT ( 'NONE',  ( 189.9621738748845132, 6.608040114328683323, 16.14673353903353004 ) ) ;
#2827 = CARTESIAN_POINT ( 'NONE',  ( -64.50000000000000000, -60.68629150101524061, -11.31370849898474873 ) ) ;
#2828 = EDGE_CURVE ( 'NONE', #7091, #1634, #2734, .T. ) ;
#2829 = CARTESIAN_POINT ( 'NONE',  ( 18.05944481925498479, -223.0630240738404382, 76.51671422530451139 ) ) ;
#2830 = CARTESIAN_POINT ( 'NONE',  ( 188.0000000000000000, -14.00000000000000711, 7.000000000000017764 ) ) ;
#2831 = CARTESIAN_POINT ( 'NONE',  ( -61.22733771064481800, -218.0630336083857230, 75.48520206723708270 ) ) ;
#2832 = AXIS2_PLACEMENT_3D ( 'NONE', #5320, #96, #1315 ) ;
#2833 = ORIENTED_EDGE ( 'NONE', *, *, #609, .T. ) ;
#2834 = CARTESIAN_POINT ( 'NONE',  ( -21.49999999999999645, -219.7493155748557285, 95.50692968358183066 ) ) ;
#2835 = DIRECTION ( 'NONE',  ( 1.000000000000000000, 0.000000000000000000, 0.000000000000000000 ) ) ;
#2836 = LINE ( 'NONE', #843, #5346 ) ;
#2837 = DIRECTION ( 'NONE',  ( 0.000000000000000000, 0.08715574274766287044, -0.9961946980917452121 ) ) ;
#2838 = VECTOR ( 'NONE', #2195, 1000.000000000000000 ) ;
#2839 = CARTESIAN_POINT ( 'NONE',  ( 186.9059892324149814, -9.000000000000000000, 14.99999999999999289 ) ) ;
#2840 = ORIENTED_EDGE ( 'NONE', *, *, #2215, .T. ) ;
#2841 = EDGE_CURVE ( 'NONE', #5002, #6433, #3864, .T. ) ;
#2842 = VECTOR ( 'NONE', #7154, 1000.000000000000000 ) ;
#2843 = EDGE_LOOP ( 'NONE', ( #1425, #5633, #6457, #7046, #4589, #2645, #6226, #1713 ) ) ;
#2844 = CARTESIAN_POINT ( 'NONE',  ( -26.49999999999999645, -214.0630240738404666, 70.86973541144037370 ) ) ;
#2845 = AXIS2_PLACEMENT_3D ( 'NONE', #1435, #2521, #4874 ) ;
#2846 = CARTESIAN_POINT ( 'NONE',  ( 3.000000000000002665, -56.99999999999999289, 10.00000000000000000 ) ) ;
#2847 = EDGE_LOOP ( 'NONE', ( #2094, #6995 ) ) ;
#2848 = CARTESIAN_POINT ( 'NONE',  ( 47.00000000000000000, 0.000000000000000000, 35.00000000000000000 ) ) ;
#2849 = DIRECTION ( 'NONE',  ( 1.000000000000000000, 0.000000000000000000, 0.000000000000000000 ) ) ;
#2850 = EDGE_LOOP ( 'NONE', ( #2039, #1011, #6901, #3844 ) ) ;
#2851 = VECTOR ( 'NONE', #4347, 1000.000000000000000 ) ;
#2852 = ORIENTED_EDGE ( 'NONE', *, *, #2828, .F. ) ;
#2853 = CARTESIAN_POINT ( 'NONE',  ( 10.03180245857092423, -218.0630240738404382, 71.94153218116483117 ) ) ;
#2854 = CARTESIAN_POINT ( 'NONE',  ( 27.03121585365657609, -223.4569485227348480, 90.54948733812101125 ) ) ;
#2855 = ORIENTED_EDGE ( 'NONE', *, *, #3972, .T. ) ;
#2856 = DIRECTION ( 'NONE',  ( 0.000000000000000000, 0.000000000000000000, -1.000000000000000000 ) ) ;
#2857 = CARTESIAN_POINT ( 'NONE',  ( 185.0000000000000000, -39.99999999999999289, 0.000000000000000000 ) ) ;
#2858 = VERTEX_POINT ( 'NONE', #6162 ) ;
#2859 = ORIENTED_EDGE ( 'NONE', *, *, #1306, .F. ) ;
#2860 = ADVANCED_FACE ( 'NONE', ( #6322 ), #3232, .F. ) ;
#2861 = CARTESIAN_POINT ( 'NONE',  ( 193.5000000000000000, 39.99999999999999289, 10.00000000000000355 ) ) ;
#2862 = DIRECTION ( 'NONE',  ( -0.000000000000000000, 0.000000000000000000, 1.000000000000000000 ) ) ;
#2863 = VECTOR ( 'NONE', #1163, 1000.000000000000000 ) ;
#2864 = DIRECTION ( 'NONE',  ( 0.000000000000000000, 0.000000000000000000, -1.000000000000000000 ) ) ;
#2865 = DIRECTION ( 'NONE',  ( 4.622231866529368100E-33, -2.600005424922769496E-32, 1.000000000000000000 ) ) ;
#2866 = DIRECTION ( 'NONE',  ( 0.000000000000000000, 1.000000000000000000, 0.000000000000000000 ) ) ;
#2867 = CARTESIAN_POINT ( 'NONE',  ( 220.0000000000000000, -60.00000000000000000, 10.00000000000000000 ) ) ;
#2868 = CARTESIAN_POINT ( 'NONE',  ( -63.59366733544099048, -218.0630240738405803, 79.12540989558915783 ) ) ;
#2869 = CONICAL_SURFACE ( 'NONE', #7172, 9.999999999999998224, 0.7853981633974501664 ) ;
#2870 = EDGE_CURVE ( 'NONE', #1753, #505, #1371, .T. ) ;
#2871 = ORIENTED_EDGE ( 'NONE', *, *, #4452, .F. ) ;
#2872 = FACE_BOUND ( 'NONE', #3752, .T. ) ;
#2873 = EDGE_CURVE ( 'NONE', #3791, #1259, #36, .T. ) ;
#2874 = DIRECTION ( 'NONE',  ( 0.000000000000000000, 0.000000000000000000, 1.000000000000000000 ) ) ;
#2875 = DIRECTION ( 'NONE',  ( -0.000000000000000000, -1.000000000000000000, -0.000000000000000000 ) ) ;
#2876 = FACE_OUTER_BOUND ( 'NONE', #5262, .T. ) ;
#2877 = VECTOR ( 'NONE', #1776, 1000.000000000000000 ) ;
#2878 = AXIS2_PLACEMENT_3D ( 'NONE', #2596, #6102, #1443 ) ;
#2879 = EDGE_LOOP ( 'NONE', ( #6127, #6555, #6819, #5590 ) ) ;
#2880 = VERTEX_POINT ( 'NONE', #6650 ) ;
#2881 = VECTOR ( 'NONE', #4703, 1000.000000000000000 ) ;
#2882 = AXIS2_PLACEMENT_3D ( 'NONE', #3452, #5870, #2979 ) ;
#2883 = VECTOR ( 'NONE', #433, 1000.000000000000000 ) ;
#2884 = FACE_OUTER_BOUND ( 'NONE', #3427, .T. ) ;
#2885 = DIRECTION ( 'NONE',  ( -1.000000000000000000, -0.000000000000000000, -0.000000000000000000 ) ) ;
#2886 = EDGE_LOOP ( 'NONE', ( #1536, #5079 ) ) ;
#2887 = CARTESIAN_POINT ( 'NONE',  ( 49.39900052591036683, -24.62867772107294329, 12.93565788627303803 ) ) ;
#2888 = DIRECTION ( 'NONE',  ( 0.000000000000000000, 0.000000000000000000, -1.000000000000000000 ) ) ;
#2889 = AXIS2_PLACEMENT_3D ( 'NONE', #6773, #3357, #2159 ) ;
#2890 = CIRCLE ( 'NONE', #3638, 3.000000000000001332 ) ;
#2891 = EDGE_LOOP ( 'NONE', ( #4941, #5172, #5148 ) ) ;
#2892 = ORIENTED_EDGE ( 'NONE', *, *, #6853, .T. ) ;
#2893 = CARTESIAN_POINT ( 'NONE',  ( 50.00000000000000000, 24.00878702352406791, 10.00000000000000888 ) ) ;
#2894 = CARTESIAN_POINT ( 'NONE',  ( 17.80066350777958917, -221.4565245236572935, 95.80795668296067902 ) ) ;
#2895 = AXIS2_PLACEMENT_3D ( 'NONE', #2167, #3976, #1006 ) ;
#2896 = EDGE_LOOP ( 'NONE', ( #1155, #1455, #1005, #3898 ) ) ;
#2897 = ITEM_DEFINED_TRANSFORMATION ( 'NONE', 'NONE', #5850,  #1914 ) ;
#2898 = EDGE_CURVE ( 'NONE', #2730, #5749, #3599, .T. ) ;
#2899 = LINE ( 'NONE', #5248, #4313 ) ;
#2900 = CARTESIAN_POINT ( 'NONE',  ( 40.00000000000000000, -4.163336342344337027E-14, 10.00000000000001243 ) ) ;
#2901 = ORIENTED_EDGE ( 'NONE', *, *, #1975, .T. ) ;
#2902 = CARTESIAN_POINT ( 'NONE',  ( -19.15685424949238680, -108.6568542494921701, 36.65685424949233351 ) ) ;
#2903 = CARTESIAN_POINT ( 'NONE',  ( 6.938893903907228378E-15, 73.78679656440351664, 0.9999999999999991118 ) ) ;
#2904 = ADVANCED_FACE ( 'NONE', ( #5037 ), #6286, .T. ) ;
#2905 = CARTESIAN_POINT ( 'NONE',  ( 20.88432520271932447, -218.0630240738405519, 79.82767783018041996 ) ) ;
#2906 = DIRECTION ( 'NONE',  ( -0.000000000000000000, -0.000000000000000000, 1.000000000000000000 ) ) ;
#2907 = DIRECTION ( 'NONE',  ( 1.000000000000000000, 1.853902270198408060E-44, 1.681558157189780485E-44 ) ) ;
#2908 = VERTEX_POINT ( 'NONE', #3848 ) ;
#2909 = VECTOR ( 'NONE', #4996, 1000.000000000000000 ) ;
#2910 = ORIENTED_EDGE ( 'NONE', *, *, #3963, .T. ) ;
#2911 = CYLINDRICAL_SURFACE ( 'NONE', #4387, 4.999999999999999112 ) ;
#2912 = DIRECTION ( 'NONE',  ( -1.000000000000000000, 1.224646799147353454E-16, 0.000000000000000000 ) ) ;
#2913 = CARTESIAN_POINT ( 'NONE',  ( 10.47314606205195631, -223.0630240738404666, 96.09122589815579829 ) ) ;
#2914 = CARTESIAN_POINT ( 'NONE',  ( 187.3752131572541373, -4.201998947814849394, 15.81271967794823574 ) ) ;
#2915 = AXIS2_PLACEMENT_3D ( 'NONE', #4600, #5253, #2326 ) ;
#2916 = EDGE_CURVE ( 'NONE', #5534, #1151, #2975, .T. ) ;
#2917 = EDGE_CURVE ( 'NONE', #2583, #3515, #2037, .T. ) ;
#2918 = ORIENTED_EDGE ( 'NONE', *, *, #5003, .T. ) ;
#2919 = VERTEX_POINT ( 'NONE', #4422 ) ;
#2920 = DIRECTION ( 'NONE',  ( 1.000000000000000000, 0.000000000000000000, 7.663350976776343357E-46 ) ) ;
#2921 = LINE ( 'NONE', #3044, #6688 ) ;
#2922 = ORIENTED_EDGE ( 'NONE', *, *, #419, .F. ) ;
#2923 = CARTESIAN_POINT ( 'NONE',  ( 49.94932960940505495, -23.57319494935126514, 10.00000000000205702 ) ) ;
#2924 = ADVANCED_FACE ( 'NONE', ( #3269 ), #7305, .F. ) ;
#2925 = CARTESIAN_POINT ( 'NONE',  ( 25.00000000000002132, 28.00000000000002487, 0.000000000000000000 ) ) ;
#2926 = VERTEX_POINT ( 'NONE', #4391 ) ;
#2927 = ORIENTED_EDGE ( 'NONE', *, *, #37, .F. ) ;
#2928 = CARTESIAN_POINT ( 'NONE',  ( 217.0000000000000000, 60.00000000000000000, 2.204364238465235507E-14 ) ) ;
#2929 = CARTESIAN_POINT ( 'NONE',  ( 27.24145449743711112, -214.0092129552772633, 88.67031792470811524 ) ) ;
#2930 = ORIENTED_EDGE ( 'NONE', *, *, #4051, .F. ) ;
#2931 = APPLICATION_PROTOCOL_DEFINITION ( 'draft international standard', 'automotive_design', 1998, #1667 ) ;
#2932 = LINE ( 'NONE', #5752, #5047 ) ;
#2933 = CARTESIAN_POINT ( 'NONE',  ( -10.49999999999996803, -49.37258300203045280, -2.775557561562891351E-14 ) ) ;
#2934 = EDGE_LOOP ( 'NONE', ( #937, #3918, #5908, #998 ) ) ;
#2935 = ADVANCED_FACE ( 'NONE', ( #5616 ), #5538, .F. ) ;
#2936 = EDGE_CURVE ( 'NONE', #5543, #7540, #3809, .T. ) ;
#2937 = DIRECTION ( 'NONE',  ( -0.4999999999999960032, -0.000000000000000000, -0.8660254037844411501 ) ) ;
#2938 = CARTESIAN_POINT ( 'NONE',  ( -26.50000000000002487, 16.00000000000012079, -15.99999999999995914 ) ) ;
#2939 = SHAPE_REPRESENTATION_RELATIONSHIP ( 'NONE' , 'NONE' ,  #6715, #2344 ) ;
#2940 = FACE_OUTER_BOUND ( 'NONE', #4142, .T. ) ;
#2941 = CARTESIAN_POINT ( 'NONE',  ( 19.96154802696617736, -223.0630240738404666, 90.65370741215697592 ) ) ;
#2942 = CARTESIAN_POINT ( 'NONE',  ( -16.49999999999996447, -59.83638031753262965, 32.83638031753273623 ) ) ;
#2943 = UNCERTAINTY_MEASURE_WITH_UNIT (LENGTH_MEASURE( 1.000000000000000082E-05 ), #2743, 'distance_accuracy_value', 'NONE');
#2944 =( REPRESENTATION_RELATIONSHIP ('NONE','NONE', #4862, #2538 ) REPRESENTATION_RELATIONSHIP_WITH_TRANSFORMATION ( #4134 )SHAPE_REPRESENTATION_RELATIONSHIP( ) );
#2945 = EDGE_CURVE ( 'NONE', #2880, #7372, #873, .T. ) ;
#2946 = ORIENTED_EDGE ( 'NONE', *, *, #492, .T. ) ;
#2947 = AXIS2_PLACEMENT_3D ( 'NONE', #5722, #1019, #6339 ) ;
#2948 =( NAMED_UNIT ( * ) PLANE_ANGLE_UNIT ( ) SI_UNIT ( $, .RADIAN. ) );
#2949 = CARTESIAN_POINT ( 'NONE',  ( -18.84314575050759188, -63.34314575050751017, 36.34314575050759544 ) ) ;
#2950 = DIRECTION ( 'NONE',  ( 1.000000000000000000, 1.853902270198408060E-44, 1.681558157189780485E-44 ) ) ;
#2951 = DIRECTION ( 'NONE',  ( 0.000000000000000000, 1.000000000000000000, 0.000000000000000000 ) ) ;
#2952 = AXIS2_PLACEMENT_3D ( 'NONE', #2135, #3840, #2711 ) ;
#2953 = VECTOR ( 'NONE', #4884, 1000.000000000000000 ) ;
#2954 = ORIENTED_EDGE ( 'NONE', *, *, #6096, .T. ) ;
#2955 = VERTEX_POINT ( 'NONE', #5649 ) ;
#2956 = EDGE_CURVE ( 'NONE', #5312, #6714, #4213, .T. ) ;
#2957 = DIRECTION ( 'NONE',  ( -1.000000000000000000, -2.624548829666596736E-30, 9.231085635203017994E-31 ) ) ;
#2958 = DIRECTION ( 'NONE',  ( 0.000000000000000000, 1.000000000000000000, 0.000000000000000000 ) ) ;
#2959 = ORIENTED_EDGE ( 'NONE', *, *, #6700, .T. ) ;
#2960 = CARTESIAN_POINT ( 'NONE',  ( -60.66255603274095165, -217.0856944719846524, 71.67965750360853860 ) ) ;
#2961 = FILL_AREA_STYLE ('',( #5429 ) ) ;
#2962 = B_SPLINE_CURVE_WITH_KNOTS ( 'NONE', 3,
 ( #3420, #1094, #1173, #3456, #479, #1133, #2300, #7482, #1792, #5797, #5759, #6951, #2829, #1058, #3989, #5218, #1627, #6453, #5905, #4568, #18, #594, #1751, #5291, #2941, #2369, #6376, #4032, #4146, #6489, #4686, #1210, #3565, #2219, #4725, #6907, #6985, #518 ),
 .UNSPECIFIED., .F., .F.,
 ( 4, 1, 1, 2, 2, 1, 1, 2, 2, 2, 2, 1, 1, 2, 2, 1, 1, 2, 2, 1, 1, 2, 2, 4 ),
 ( 0.000000000000000000, 0.06249999999999945877, 0.09374999999999929223, 0.1093749999999992228, 0.1249999999999991396, 0.1874999999999995837, 0.2187499999999996392, 0.2343749999999995282, 0.2499999999999994449, 0.3749999999999973910, 0.4999999999999953926, 0.5624999999999948930, 0.5937499999999941158, 0.6093749999999936717, 0.6249999999999933387, 0.6874999999999940048, 0.7187499999999943379, 0.7343749999999946709, 0.7499999999999948930, 0.8124999999999957812, 0.8437499999999958922, 0.8593749999999960032, 0.8749999999999961142, 1.000000000000000000 ),
 .UNSPECIFIED. ) ;
#2963 = CARTESIAN_POINT ( 'NONE',  ( 220.0000000000000000, 20.99999999999999645, 13.00000000000000888 ) ) ;
#2964 = AXIS2_PLACEMENT_3D ( 'NONE', #3236, #1459, #1966 ) ;
#2965 = ORIENTED_EDGE ( 'NONE', *, *, #1452, .F. ) ;
#2966 = VERTEX_POINT ( 'NONE', #6114 ) ;
#2967 = VECTOR ( 'NONE', #6829, 1000.000000000000000 ) ;
#2968 = EDGE_CURVE ( 'NONE', #1233, #3466, #878, .T. ) ;
#2969 = DIRECTION ( 'NONE',  ( 0.000000000000000000, 0.000000000000000000, -1.000000000000000000 ) ) ;
#2970 = CARTESIAN_POINT ( 'NONE',  ( 17.81252276423129999, -222.2597742987536265, 95.94959129056174163 ) ) ;
#2971 = VERTEX_POINT ( 'NONE', #340 ) ;
#2972 = APPLICATION_PROTOCOL_DEFINITION ( 'draft international standard', 'automotive_design', 1998, #1270 ) ;
#2973 = CYLINDRICAL_SURFACE ( 'NONE', #2233, 13.99999999999999112 ) ;
#2974 = FACE_OUTER_BOUND ( 'NONE', #7115, .T. ) ;
#2975 = CIRCLE ( 'NONE', #5558, 2.999999999999999112 ) ;
#2976 = VERTEX_POINT ( 'NONE', #1373 ) ;
#2977 = DIRECTION ( 'NONE',  ( 1.000000000000000000, -5.551115123125783935E-17, 4.237045877651920245E-33 ) ) ;
#2978 = AXIS2_PLACEMENT_3D ( 'NONE', #5231, #7566, #7458 ) ;
#2979 = DIRECTION ( 'NONE',  ( 1.000000000000000000, 0.000000000000000000, 0.000000000000000000 ) ) ;
#2980 = CARTESIAN_POINT ( 'NONE',  ( 17.59106180226908478, -218.0630240738404950, 74.83367537032552264 ) ) ;
#2981 = CARTESIAN_POINT ( 'NONE',  ( 3.000000000000002665, 0.000000000000000000, 35.00000000000000000 ) ) ;
#2982 = DIRECTION ( 'NONE',  ( 0.000000000000000000, 0.000000000000000000, -1.000000000000000000 ) ) ;
#2983 = EDGE_CURVE ( 'NONE', #6591, #628, #1956, .T. ) ;
#2984 =( BOUNDED_CURVE ( )  B_SPLINE_CURVE ( 3, ( #5535, #6071, #4198, #6543 ),
 .UNSPECIFIED., .F., .T. ) 
 B_SPLINE_CURVE_WITH_KNOTS ( ( 4, 4 ),
 ( 3.141592653589793116, 4.712388980384689674 ),
 .UNSPECIFIED. ) 
 CURVE ( )  GEOMETRIC_REPRESENTATION_ITEM ( )  RATIONAL_B_SPLINE_CURVE ( ( 1.000000000000000000, 0.8047378541243649375, 0.8047378541243649375, 1.000000000000000000 ) ) 
 REPRESENTATION_ITEM ( '' )  );
#2985 = EDGE_LOOP ( 'NONE', ( #6006, #2082, #7148, #4261, #5998 ) ) ;
#2986 = AXIS2_PLACEMENT_3D ( 'NONE', #6326, #2251, #2736 ) ;
#2987 = CARTESIAN_POINT ( 'NONE',  ( 6.500000000000007994, 12.50000000000001243, -1.214306433183764966E-14 ) ) ;
#2988 = CYLINDRICAL_SURFACE ( 'NONE', #5672, 13.99999999999999645 ) ;
#2989 = DIRECTION ( 'NONE',  ( -0.8660254037844413721, 0.000000000000000000, 0.4999999999999950595 ) ) ;
#2990 = CARTESIAN_POINT ( 'NONE',  ( 25.00000000000000711, 28.00000000000002487, 9.999999999999996447 ) ) ;
#2991 = LINE ( 'NONE', #7033, #3719 ) ;
#2992 = EDGE_CURVE ( 'NONE', #5355, #4160, #3735, .T. ) ;
#2993 = AXIS2_PLACEMENT_3D ( 'NONE', #935, #5788, #3364 ) ;
#2994 = CIRCLE ( 'NONE', #1392, 9.999999999999998224 ) ;
#2995 = EDGE_LOOP ( 'NONE', ( #6406, #2420, #5817, #5603 ) ) ;
#2996 = ORIENTED_EDGE ( 'NONE', *, *, #3731, .F. ) ;
#2997 = DIRECTION ( 'NONE',  ( 5.605193857299270773E-45, 0.000000000000000000, 1.000000000000000000 ) ) ;
#2998 = VECTOR ( 'NONE', #1613, 1000.000000000000000 ) ;
#2999 = DIRECTION ( 'NONE',  ( 5.605193857299270773E-45, 0.000000000000000000, 1.000000000000000000 ) ) ;
#3000 = ORIENTED_EDGE ( 'NONE', *, *, #5809, .F. ) ;
#3001 = CARTESIAN_POINT ( 'NONE',  ( -70.21559789597881718, -217.6453243769069559, 77.74120035865658451 ) ) ;
#3002 = EDGE_CURVE ( 'NONE', #2575, #687, #5576, .T. ) ;
#3003 = DIRECTION ( 'NONE',  ( 1.000000000000000000, 0.000000000000000000, 0.000000000000000000 ) ) ;
#3004 = DIRECTION ( 'NONE',  ( 1.000000000000000000, 2.465190328815661892E-32, -9.244463733058732095E-33 ) ) ;
#3005 = EDGE_CURVE ( 'NONE', #5964, #578, #7266, .T. ) ;
#3006 = ORIENTED_EDGE ( 'NONE', *, *, #1153, .T. ) ;
#3007 = CIRCLE ( 'NONE', #2146, 6.000000000000001776 ) ;
#3008 = AXIS2_PLACEMENT_3D ( 'NONE', #4218, #172, #244 ) ;
#3009 = VECTOR ( 'NONE', #4833, 1000.000000000000114 ) ;
#3010 = EDGE_LOOP ( 'NONE', ( #6344, #3292, #4287, #926 ) ) ;
#3011 = DIRECTION ( 'NONE',  ( -1.000000000000000000, 5.551115123125783935E-17, -4.237045877651919561E-33 ) ) ;
#3012 = CARTESIAN_POINT ( 'NONE',  ( 10.40199052334513041, -226.2606222968796601, 74.13807200490302307 ) ) ;
#3013 = ORIENTED_EDGE ( 'NONE', *, *, #4411, .T. ) ;
#3014 = APPLICATION_PROTOCOL_DEFINITION ( 'draft international standard', 'automotive_design', 1998, #3644 ) ;
#3015 = AXIS2_PLACEMENT_3D ( 'NONE', #455, #2268, #1104 ) ;
#3016 = CYLINDRICAL_SURFACE ( 'NONE', #5169, 3.000000000000000888 ) ;
#3017 = VECTOR ( 'NONE', #1171, 999.9999999999998863 ) ;
#3018 = FACE_OUTER_BOUND ( 'NONE', #1236, .T. ) ;
#3019 = EDGE_CURVE ( 'NONE', #5363, #4861, #2685, .T. ) ;
#3020 = ADVANCED_FACE ( 'NONE', ( #5008 ), #2072, .F. ) ;
#3021 = ORIENTED_EDGE ( 'NONE', *, *, #5199, .T. ) ;
#3022 = PRODUCT_RELATED_PRODUCT_CATEGORY ( 'part', '', ( #5056 ) ) ;
#3023 = ORIENTED_EDGE ( 'NONE', *, *, #4052, .F. ) ;
#3024 = FACE_OUTER_BOUND ( 'NONE', #3717, .T. ) ;
#3025 = CARTESIAN_POINT ( 'NONE',  ( 2.000000000000001776, 0.000000000000000000, -10.00000000000000355 ) ) ;
#3026 = DIRECTION ( 'NONE',  ( -0.000000000000000000, -0.000000000000000000, 1.000000000000000000 ) ) ;
#3027 = CARTESIAN_POINT ( 'NONE',  ( 15.61587190384303980, -218.0630240738405519, 73.42250040783586940 ) ) ;
#3028 = DIRECTION ( 'NONE',  ( 0.000000000000000000, 0.000000000000000000, 1.000000000000000000 ) ) ;
#3029 = UNCERTAINTY_MEASURE_WITH_UNIT (LENGTH_MEASURE( 1.000000000000000082E-05 ), #1374, 'distance_accuracy_value', 'NONE');
#3030 = VECTOR ( 'NONE', #6038, 1000.000000000000000 ) ;
#3031 = DIRECTION ( 'NONE',  ( 0.000000000000000000, 0.000000000000000000, 1.000000000000000000 ) ) ;
#3032 = CYLINDRICAL_SURFACE ( 'NONE', #4851, 8.000000000000007105 ) ;
#3033 = CARTESIAN_POINT ( 'NONE',  ( -2.354181420065692281E-43, -1.853902270198407045E-42, 13.99999999999999822 ) ) ;
#3034 = DIRECTION ( 'NONE',  ( 1.000000000000000000, 0.000000000000000000, 0.000000000000000000 ) ) ;
#3035 = DIRECTION ( 'NONE',  ( 1.000000000000000000, 0.000000000000000000, 5.605193857299269528E-45 ) ) ;
#3036 = LINE ( 'NONE', #5383, #5042 ) ;
#3037 =( BOUNDED_CURVE ( )  B_SPLINE_CURVE ( 3, ( #5153, #3924, #6422, #1639 ),
 .UNSPECIFIED., .F., .T. ) 
 B_SPLINE_CURVE_WITH_KNOTS ( ( 4, 4 ),
 ( 1.570796326794896558, 2.443460952792054552 ),
 .UNSPECIFIED. ) 
 CURVE ( )  GEOMETRIC_REPRESENTATION_ITEM ( )  RATIONAL_B_SPLINE_CURVE ( ( 1.000000000000000000, 0.9375385246911008830, 0.9375385246911008830, 1.000000000000000000 ) ) 
 REPRESENTATION_ITEM ( '' )  );
#3038 = VECTOR ( 'NONE', #5490, 1000.000000000000114 ) ;
#3039 = ORIENTED_EDGE ( 'NONE', *, *, #1908, .F. ) ;
#3040 = ORIENTED_EDGE ( 'NONE', *, *, #5413, .T. ) ;
#3041 = EDGE_CURVE ( 'NONE', #4710, #3465, #4042, .T. ) ;
#3042 = FACE_OUTER_BOUND ( 'NONE', #7596, .T. ) ;
#3043 = CIRCLE ( 'NONE', #4777, 8.000000000000007105 ) ;
#3044 = CARTESIAN_POINT ( 'NONE',  ( 26.37580566599013920, -63.12419433401035462, -8.875805665989638271 ) ) ;
#3045 = EDGE_LOOP ( 'NONE', ( #739, #1693, #3703, #4071 ) ) ;
#3046 = PRODUCT ( 'base', 'base', '', ( #2290 ) ) ;
#3047 = CARTESIAN_POINT ( 'NONE',  ( -60.73846410710429211, -222.1285142276679778, 73.03087698472576506 ) ) ;
#3048 = CARTESIAN_POINT ( 'NONE',  ( 47.81196995442319064, -25.80454930986227424, 9.999999999997962519 ) ) ;
#3049 = CARTESIAN_POINT ( 'NONE',  ( 217.0000000000000000, 20.99999999999999645, 7.000000000000009770 ) ) ;
#3050 = ORIENTED_EDGE ( 'NONE', *, *, #5562, .F. ) ;
#3051 = AXIS2_PLACEMENT_3D ( 'NONE', #5352, #6965, #3434 ) ;
#3052 = ORIENTED_EDGE ( 'NONE', *, *, #5811, .T. ) ;
#3053 = EDGE_CURVE ( 'NONE', #191, #6725, #5119, .T. ) ;
#3054 = CARTESIAN_POINT ( 'NONE',  ( 50.00000000000000000, -22.78166690339260825, 13.00000000000000711 ) ) ;
#3055 = CARTESIAN_POINT ( 'NONE',  ( 27.19709702122541017, -218.4687108041559895, 77.94269080187306997 ) ) ;
#3056 = ORIENTED_EDGE ( 'NONE', *, *, #2898, .F. ) ;
#3057 = CARTESIAN_POINT ( 'NONE',  ( 26.00000000000000000, 0.000000000000000000, 0.000000000000000000 ) ) ;
#3058 = DIRECTION ( 'NONE',  ( -4.336808689942025132E-16, 3.989863994746663259E-14, 1.000000000000000000 ) ) ;
#3059 = ORIENTED_EDGE ( 'NONE', *, *, #3135, .T. ) ;
#3060 = DIRECTION ( 'NONE',  ( -5.605193857299269528E-45, 0.000000000000000000, 1.000000000000000000 ) ) ;
#3061 = EDGE_CURVE ( 'NONE', #3465, #6591, #3037, .T. ) ;
#3062 = CARTESIAN_POINT ( 'NONE',  ( 1.387778780781445676E-14, 101.5000000000000000, -1.734723475976807094E-15 ) ) ;
#3063 = ORIENTED_EDGE ( 'NONE', *, *, #921, .F. ) ;
#3064 =( NAMED_UNIT ( * ) PLANE_ANGLE_UNIT ( ) SI_UNIT ( $, .RADIAN. ) );
#3065 = CARTESIAN_POINT ( 'NONE',  ( 25.00000000000002132, 82.46446609406720540, 6.464466094067254254 ) ) ;
#3066 = LINE ( 'NONE', #1249, #5412 ) ;
#3067 = CARTESIAN_POINT ( 'NONE',  ( 50.04196010845020481, 18.04196010845019060, 12.50000000000000711 ) ) ;
#3068 = DIRECTION ( 'NONE',  ( 2.627434620609032786E-46, -0.7071067811865464625, 0.7071067811865485719 ) ) ;
#3069 = ADVANCED_FACE ( 'NONE', ( #2876 ), #3391, .F. ) ;
#3070 = LINE ( 'NONE', #1295, #2140 ) ;
#3071 = CARTESIAN_POINT ( 'NONE',  ( 217.0000000000000000, -60.00000000000000000, 3.000000000000000444 ) ) ;
#3072 = DIRECTION ( 'NONE',  ( -1.000000000000000000, 5.551115123125783935E-17, -4.237045877651919561E-33 ) ) ;
#3073 = CARTESIAN_POINT ( 'NONE',  ( 188.5076150991777411, 8.869380270722979631, 15.00000000000000533 ) ) ;
#3074 = CARTESIAN_POINT ( 'NONE',  ( 189.2293793704153018, -5.809691905097411180, 19.02422976478239391 ) ) ;
#3075 = VECTOR ( 'NONE', #3867, 1000.000000000000227 ) ;
#3076 = ORIENTED_EDGE ( 'NONE', *, *, #4645, .T. ) ;
#3077 = ORIENTED_EDGE ( 'NONE', *, *, #4305, .F. ) ;
#3078 = CARTESIAN_POINT ( 'NONE',  ( 25.00000000000001421, 80.85786437626907741, 8.071067811865434649 ) ) ;
#3079 = DIRECTION ( 'NONE',  ( -1.000000000000000000, 0.000000000000000000, 0.000000000000000000 ) ) ;
#3080 = VECTOR ( 'NONE', #4301, 1000.000000000000000 ) ;
#3081 = CARTESIAN_POINT ( 'NONE',  ( -60.67236366837565953, -217.7372475398859706, 71.85424062197719763 ) ) ;
#3082 = CARTESIAN_POINT ( 'NONE',  ( 30.00000000000000000, 0.000000000000000000, 10.00000000000000355 ) ) ;
#3083 = CARTESIAN_POINT ( 'NONE',  ( -61.07266449636613004, -218.0629854895634594, 91.98311311191383766 ) ) ;
#3084 = EDGE_CURVE ( 'NONE', #6198, #1926, #7271, .T. ) ;
#3085 = ADVANCED_FACE ( 'NONE', ( #2190 ), #6385, .F. ) ;
#3086 = ORIENTED_EDGE ( 'NONE', *, *, #7167, .F. ) ;
#3087 = EDGE_LOOP ( 'NONE', ( #3000, #4896, #337, #3473 ) ) ;
#3088 = DIRECTION ( 'NONE',  ( 0.000000000000000000, -1.000000000000000000, -2.065146995210484941E-16 ) ) ;
#3089 = CARTESIAN_POINT ( 'NONE',  ( 9.987668098222851398, -217.0856944719845387, 71.67965750360849597 ) ) ;
#3090 = ORIENTED_EDGE ( 'NONE', *, *, #1788, .T. ) ;
#3091 = DIRECTION ( 'NONE',  ( 0.000000000000000000, 1.000000000000000000, 0.000000000000000000 ) ) ;
#3092 = CARTESIAN_POINT ( 'NONE',  ( 2.000000000000001776, -4.163336342344337027E-14, 0.000000000000000000 ) ) ;
#3093 = EDGE_LOOP ( 'NONE', ( #858, #4496, #3358, #136 ) ) ;
#3094 = DIRECTION ( 'NONE',  ( -1.000000000000000000, -0.000000000000000000, -0.000000000000000000 ) ) ;
#3095 = DIRECTION ( 'NONE',  ( -0.000000000000000000, -1.000000000000000000, -1.836970198721029934E-16 ) ) ;
#3096 = APPLICATION_CONTEXT ( 'automotive_design' ) ;
#3097 = VECTOR ( 'NONE', #3207, 1000.000000000000000 ) ;
#3098 = CARTESIAN_POINT ( 'NONE',  ( 24.99999999999999289, 86.00000000000001421, -1.214306433183764966E-14 ) ) ;
#3099 = FACE_OUTER_BOUND ( 'NONE', #4200, .T. ) ;
#3100 = EDGE_CURVE ( 'NONE', #3854, #7274, #2112, .T. ) ;
#3101 = EDGE_CURVE ( 'NONE', #5579, #1932, #4504, .T. ) ;
#3102 = VECTOR ( 'NONE', #4659, 1000.000000000000114 ) ;
#3103 = CARTESIAN_POINT ( 'NONE',  ( 12.50000000000001066, 12.50000000000001066, 4.999999999999995559 ) ) ;
#3104 = FILL_AREA_STYLE_COLOUR ( '', #540 ) ;
#3105 = CARTESIAN_POINT ( 'NONE',  ( -21.50000000000000000, -114.3401965514817817, 42.31370849898471675 ) ) ;
#3106 = CARTESIAN_POINT ( 'NONE',  ( -64.26447795140279595, -223.0648723219386511, 82.43246165033174577 ) ) ;
#3107 = CARTESIAN_POINT ( 'NONE',  ( -69.37580566599014276, -63.12419433401035462, -8.875805665989638271 ) ) ;
#3108 = EDGE_CURVE ( 'NONE', #1936, #3466, #2803, .T. ) ;
#3109 = ORIENTED_EDGE ( 'NONE', *, *, #6184, .T. ) ;
#3110 = ORIENTED_EDGE ( 'NONE', *, *, #3842, .F. ) ;
#3111 = DIRECTION ( 'NONE',  ( -5.551115123125785167E-17, 0.7071067811865452413, -0.7071067811865499042 ) ) ;
#3112 = CARTESIAN_POINT ( 'NONE',  ( 170.0000000000000000, 11.00000000000000711, 8.660254037844383745 ) ) ;
#3113 = CARTESIAN_POINT ( 'NONE',  ( -70.03121585365657609, -225.8512969706634408, 79.74927943323393720 ) ) ;
#3114 = CIRCLE ( 'NONE', #1015, 2.999999999999999112 ) ;
#3115 = CARTESIAN_POINT ( 'NONE',  ( -64.50000000000000000, -39.68629150101521219, 16.00000000000001421 ) ) ;
#3116 = CARTESIAN_POINT ( 'NONE',  ( -57.62345916743081631, -218.0630240738404950, 94.30959155535899185 ) ) ;
#3117 = ORIENTED_EDGE ( 'NONE', *, *, #2285, .F. ) ;
#3118 = ORIENTED_EDGE ( 'NONE', *, *, #1053, .T. ) ;
#3119 = VECTOR ( 'NONE', #4750, 1000.000000000000000 ) ;
#3120 = VECTOR ( 'NONE', #6381, 1000.000000000000000 ) ;
#3121 = CARTESIAN_POINT ( 'NONE',  ( 27.10306686690893940, -222.6535482193571909, 78.96676008164924099 ) ) ;
#3122 = EDGE_LOOP ( 'NONE', ( #2927, #6139, #4922, #4547 ) ) ;
#3123 = DIRECTION ( 'NONE',  ( 0.000000000000000000, 0.000000000000000000, -1.000000000000000000 ) ) ;
#3124 = DIRECTION ( 'NONE',  ( 0.000000000000000000, 0.000000000000000000, -1.000000000000000000 ) ) ;
#3125 = VECTOR ( 'NONE', #2355, 1000.000000000000000 ) ;
#3126 = CONICAL_SURFACE ( 'NONE', #5466, 7.999999999999986677, 0.7853981633974473908 ) ;
#3127 = ORIENTED_EDGE ( 'NONE', *, *, #3553, .F. ) ;
#3128 = CARTESIAN_POINT ( 'NONE',  ( -13.49999999999999822, -223.0630240738404382, 73.28127814332047762 ) ) ;
#3129 = CIRCLE ( 'NONE', #5344, 3.000000000000000000 ) ;
#3130 = EDGE_CURVE ( 'NONE', #3448, #1532, #4829, .T. ) ;
#3131 = AXIS2_PLACEMENT_3D ( 'NONE', #6409, #4797, #2296 ) ;
#3132 = DIRECTION ( 'NONE',  ( -1.000000000000000000, 1.294224922628222493E-31, -1.078147950931789264E-16 ) ) ;
#3133 = AXIS2_PLACEMENT_3D ( 'NONE', #5298, #6460, #601 ) ;
#3134 = ORIENTED_EDGE ( 'NONE', *, *, #2956, .F. ) ;
#3135 = EDGE_CURVE ( 'NONE', #5312, #6160, #3346, .T. ) ;
#3136 = CARTESIAN_POINT ( 'NONE',  ( 37.99999999999998579, -4.163336342344337027E-14, 10.00000000000001243 ) ) ;
#3137 = CARTESIAN_POINT ( 'NONE',  ( -16.50000000000000000, -104.1739323729103717, 75.12787131935894536 ) ) ;
#3138 = DIRECTION ( 'NONE',  ( 0.000000000000000000, 0.000000000000000000, -1.000000000000000000 ) ) ;
#3139 = CIRCLE ( 'NONE', #7072, 13.99999999999999112 ) ;
#3140 = DIRECTION ( 'NONE',  ( 1.000000000000000000, 2.624548829666596385E-30, 9.231085635203014490E-31 ) ) ;
#3141 = ORIENTED_EDGE ( 'NONE', *, *, #1037, .F. ) ;
#3142 = SURFACE_STYLE_USAGE ( .BOTH. , #3686 ) ;
#3143 = DIRECTION ( 'NONE',  ( 0.000000000000000000, 0.000000000000000000, -1.000000000000000000 ) ) ;
#3144 = CARTESIAN_POINT ( 'NONE',  ( -64.51262296323307055, -223.0630240738404098, 85.62222623059837190 ) ) ;
#3145 = DIRECTION ( 'NONE',  ( 0.000000000000000000, 0.000000000000000000, -1.000000000000000000 ) ) ;
#3146 = ORIENTED_EDGE ( 'NONE', *, *, #4523, .T. ) ;
#3147 = VERTEX_POINT ( 'NONE', #5691 ) ;
#3148 = CARTESIAN_POINT ( 'NONE',  ( -53.06880420804609599, -218.8824061789517259, 72.16108495452195370 ) ) ;
#3149 = CARTESIAN_POINT ( 'NONE',  ( 3.000000000000002665, 27.04312195450891565, 12.73853277175702559 ) ) ;
#3150 = ADVANCED_FACE ( 'NONE', ( #3961 ), #1068, .F. ) ;
#3151 = EDGE_CURVE ( 'NONE', #3744, #5755, #6842, .T. ) ;
#3152 = DIRECTION ( 'NONE',  ( 0.000000000000000000, 0.000000000000000000, 1.000000000000000000 ) ) ;
#3153 = VECTOR ( 'NONE', #4849, 1000.000000000000000 ) ;
#3154 = CARTESIAN_POINT ( 'NONE',  ( -16.49999999999996447, -60.68629150101523351, -11.31370849898472031 ) ) ;
#3155 = CARTESIAN_POINT ( 'NONE',  ( -64.47552857335868737, -218.0623681019555420, 84.48708328684777769 ) ) ;
#3156 = ORIENTED_EDGE ( 'NONE', *, *, #2447, .T. ) ;
#3157 = ORIENTED_EDGE ( 'NONE', *, *, #3333, .F. ) ;
#3158 = CIRCLE ( 'NONE', #6966, 3.000000000000000444 ) ;
#3159 = DIRECTION ( 'NONE',  ( 1.000000000000000000, 0.000000000000000000, 0.000000000000000000 ) ) ;
#3160 = DIRECTION ( 'NONE',  ( 1.000000000000000000, 0.000000000000000000, 0.000000000000000000 ) ) ;
#3161 = ADVANCED_FACE ( 'NONE', ( #4579 ), #5073, .T. ) ;
#3162 = VERTEX_POINT ( 'NONE', #3431 ) ;
#3163 = CONTEXT_DEPENDENT_SHAPE_REPRESENTATION ( #2593, #3618 ) ;
#3164 = DIRECTION ( 'NONE',  ( 1.000000000000000000, 0.000000000000000000, 0.000000000000000000 ) ) ;
#3165 = DIRECTION ( 'NONE',  ( -1.000000000000000000, 0.000000000000000000, -7.663350976776343357E-46 ) ) ;
#3166 = AXIS2_PLACEMENT_3D ( 'NONE', #2047, #4401, #1462 ) ;
#3167 = EDGE_LOOP ( 'NONE', ( #4980, #2852, #4599, #2737 ) ) ;
#3168 = DIRECTION ( 'NONE',  ( 0.000000000000000000, -1.000000000000000000, -1.221245327087672392E-15 ) ) ;
#3169 = DIRECTION ( 'NONE',  ( -1.000000000000000000, 0.000000000000000000, 0.000000000000000000 ) ) ;
#3170 = ORIENTED_EDGE ( 'NONE', *, *, #6654, .F. ) ;
#3171 = CARTESIAN_POINT ( 'NONE',  ( 21.50000000000000000, -39.68629150101520509, 23.99999999999999289 ) ) ;
#3172 = CARTESIAN_POINT ( 'NONE',  ( -26.50000000000003197, -39.68629150101522640, 24.00000000000002132 ) ) ;
#3173 = DIRECTION ( 'NONE',  ( 1.000000000000000000, 2.624548829666596736E-30, -9.231085635203017994E-31 ) ) ;
#3174 = VERTEX_POINT ( 'NONE', #2151 ) ;
#3175 = ADVANCED_FACE ( 'NONE', ( #412 ), #672, .T. ) ;
#3176 = B_SPLINE_CURVE_WITH_KNOTS ( 'NONE', 3,
 ( #3105, #3259, #752, #5454 ),
 .UNSPECIFIED., .F., .F.,
 ( 4, 4 ),
 ( 5.887846720064191696E-17, 0.0007743866022177889373 ),
 .UNSPECIFIED. ) ;
#3177 = LINE ( 'NONE', #5525, #4392 ) ;
#3178 = FILL_AREA_STYLE ('',( #3104 ) ) ;
#3179 = FACE_OUTER_BOUND ( 'NONE', #22, .T. ) ;
#3180 = CARTESIAN_POINT ( 'NONE',  ( -64.00645916684678127, -223.0646730209604698, 81.35415196545162075 ) ) ;
#3181 = EDGE_LOOP ( 'NONE', ( #7210, #297, #4462 ) ) ;
#3182 = CARTESIAN_POINT ( 'NONE',  ( 0.000000000000000000, 24.95512646718981742, 2.183290662734949983 ) ) ;
#3183 = ORIENTED_EDGE ( 'NONE', *, *, #7228, .F. ) ;
#3184 = ORIENTED_EDGE ( 'NONE', *, *, #5294, .F. ) ;
#3185 = DIRECTION ( 'NONE',  ( 1.000000000000000000, -5.551115123125783935E-17, 4.237045877651919561E-33 ) ) ;
#3186 = CARTESIAN_POINT ( 'NONE',  ( 43.50000000000001421, 39.99999999999999289, 10.00000000000000355 ) ) ;
#3187 = DIRECTION ( 'NONE',  ( -1.000000000000000000, -2.624548829666596736E-30, 9.231085635203017994E-31 ) ) ;
#3188 = DIRECTION ( 'NONE',  ( -1.681558157189779738E-44, 0.000000000000000000, -1.000000000000000000 ) ) ;
#3189 = ORIENTED_EDGE ( 'NONE', *, *, #7247, .F. ) ;
#3190 = ADVANCED_FACE ( 'NONE', ( #1758, #150 ), #6610, .F. ) ;
#3191 = ORIENTED_EDGE ( 'NONE', *, *, #7105, .F. ) ;
#3192 = CIRCLE ( 'NONE', #4188, 8.500000000000007105 ) ;
#3193 = AXIS2_PLACEMENT_3D ( 'NONE', #6058, #782, #3138 ) ;
#3194 = DIRECTION ( 'NONE',  ( 1.000000000000000000, 1.853902270198408060E-44, 1.681558157189780485E-44 ) ) ;
#3195 = CARTESIAN_POINT ( 'NONE',  ( 36.00000000000000000, 0.000000000000000000, 1.387778780781445676E-14 ) ) ;
#3196 = ORIENTED_EDGE ( 'NONE', *, *, #4452, .T. ) ;
#3197 = DIRECTION ( 'NONE',  ( 0.000000000000000000, 0.1666666666666668239, -0.9860132971832694659 ) ) ;
#3198 = DIRECTION ( 'NONE',  ( 0.000000000000000000, 0.000000000000000000, -1.000000000000000000 ) ) ;
#3199 = ORIENTED_EDGE ( 'NONE', *, *, #5889, .T. ) ;
#3200 = EDGE_CURVE ( 'NONE', #5898, #3265, #1489, .T. ) ;
#3201 = EDGE_CURVE ( 'NONE', #5278, #452, #2991, .T. ) ;
#3202 = CYLINDRICAL_SURFACE ( 'NONE', #705, 5.999999999999999112 ) ;
#3203 = VECTOR ( 'NONE', #1570, 1000.000000000000000 ) ;
#3204 = CARTESIAN_POINT ( 'NONE',  ( 47.00000000000000000, 27.28271252673189551, 10.00000000000000711 ) ) ;
#3205 = DIRECTION ( 'NONE',  ( -0.000000000000000000, -0.000000000000000000, 1.000000000000000000 ) ) ;
#3206 = EDGE_LOOP ( 'NONE', ( #5928, #4434, #1817, #462, #3684, #2242, #5628, #341 ) ) ;
#3207 = DIRECTION ( 'NONE',  ( -1.000000000000000000, 0.000000000000000000, -7.663350976776343357E-46 ) ) ;
#3208 = LINE ( 'NONE', #354, #4690 ) ;
#3209 = CARTESIAN_POINT ( 'NONE',  ( 217.0000000000000000, -60.00000000000000000, 7.000000000000000888 ) ) ;
#3210 = PRODUCT ( 'link', 'link', '', ( #4757 ) ) ;
#3211 = VERTEX_POINT ( 'NONE', #6463 ) ;
#3212 = VECTOR ( 'NONE', #7383, 1000.000000000000000 ) ;
#3213 = ORIENTED_EDGE ( 'NONE', *, *, #3151, .T. ) ;
#3214 = DIRECTION ( 'NONE',  ( 0.000000000000000000, 0.9961946980917452121, 0.08715574274766277330 ) ) ;
#3215 = VECTOR ( 'NONE', #717, 1000.000000000000000 ) ;
#3216 = CARTESIAN_POINT ( 'NONE',  ( 25.00000000000000000, 73.78679656440354506, 5.999999999999996447 ) ) ;
#3217 = CARTESIAN_POINT ( 'NONE',  ( -64.50000000000000000, -49.37258300203048123, -15.99999999999998579 ) ) ;
#3218 = ADVANCED_FACE ( 'NONE', ( #1219 ), #1181, .T. ) ;
#3219 = CARTESIAN_POINT ( 'NONE',  ( -60.04440983696338918, -223.0634580850465625, 75.61957205288878470 ) ) ;
#3220 = CYLINDRICAL_SURFACE ( 'NONE', #1232, 8.500000000000007105 ) ;
#3221 = DIRECTION ( 'NONE',  ( -1.000000000000000000, 5.551115123125783935E-17, -4.237045877651919561E-33 ) ) ;
#3222 = AXIS2_PLACEMENT_3D ( 'NONE', #1541, #2124, #2205 ) ;
#3223 = ORIENTED_EDGE ( 'NONE', *, *, #971, .F. ) ;
#3224 = VERTEX_POINT ( 'NONE', #4228 ) ;
#3225 = LINE ( 'NONE', #4961, #5980 ) ;
#3226 = EDGE_CURVE ( 'NONE', #1532, #3586, #2377, .T. ) ;
#3227 = CARTESIAN_POINT ( 'NONE',  ( 3.000000000000002665, 21.91628335801839356, 36.91742634044857141 ) ) ;
#3228 = DIRECTION ( 'NONE',  ( 1.000000000000000000, 2.624548829666596736E-30, -9.231085635203017994E-31 ) ) ;
#3229 = PRODUCT_DEFINITION_CONTEXT ( 'detailed design', #2555, 'design' ) ;
#3230 = ORIENTED_EDGE ( 'NONE', *, *, #3899, .T. ) ;
#3231 = ORIENTED_EDGE ( 'NONE', *, *, #4350, .F. ) ;
#3232 =( BOUNDED_SURFACE ( )  B_SPLINE_SURFACE ( 5, 3, ( 
 ( #3248, #393, #2817, #7438, #7508, #1618, #469, #6200, #5629, #890, #5021, #2700, #5132, #5053, #2089, #5092 ),
 ( #1466, #1048, #7392, #7355, #353, #4440, #2665, #5599, #6821, #3977, #3408, #4477, #2249, #323, #3906, #6240 ),
 ( #968, #2168, #6280, #1008, #3362, #1845, #6615, #7082, #3698, #6469, #1880, #2460, #1228, #5391, #121, #4816 ),
 ( #6938, #6548, #1922, #3113, #4748, #158, #3624, #7153, #5428, #1811, #5887, #4125, #3001, #4274, #613, #3587 ),
 ( #4165, #6507, #5965, #692, #6040, #5925, #1189, #762, #4237, #3047, #651, #3548, #5356, #3081, #4201, #2960 ),
 ( #2495, #5467, #84, #2425, #1337, #1265, #4783, #7119, #6582, #1304, #198, #7193, #4595, #3665, #5309, #1768 ) ),
 .UNSPECIFIED., .F., .F., .T. ) 
 B_SPLINE_SURFACE_WITH_KNOTS ( ( 6, 6 ),
 ( 4, 2, 2, 2, 2, 2, 2, 4 ),
 ( 0.000000000000000000, 1.000000000000000000 ),
 ( -1.150125124083905659, -0.9546592037126467867, -0.4819498650540673390, 0.000000000000000000, 0.02616758540912784634, 0.5083707369372295615, 0.9999999999999414912, 1.195465920371200363 ),
 .UNSPECIFIED. ) 
 GEOMETRIC_REPRESENTATION_ITEM ( )  RATIONAL_B_SPLINE_SURFACE ( (
 ( 1.000000000000000000, 1.000000000000000000, 1.000000000000000000, 1.000000000000000000, 1.000000000000000000, 1.000000000000000000, 1.000000000000000000, 1.000000000000000000, 1.000000000000000000, 1.000000000000000000, 1.000000000000000000, 1.000000000000000000, 1.000000000000000000, 1.000000000000000000, 1.000000000000000000, 1.000000000000000000),
 ( 0.5999999999999995337, 0.5999999999999995337, 0.5999999999999999778, 0.5999999999999999778, 0.5999999999999999778, 0.5999999999999999778, 0.5999999999999999778, 0.5999999999999999778, 0.5999999999999995337, 0.5999999999999995337, 0.5999999999999999778, 0.5999999999999999778, 0.5999999999999989786, 0.5999999999999989786, 0.5999999999999995337, 0.5999999999999995337),
 ( 0.3999999999999993561, 0.3999999999999993561, 0.4000000000000000777, 0.4000000000000000777, 0.4000000000000000777, 0.4000000000000000777, 0.4000000000000000777, 0.4000000000000000777, 0.3999999999999993561, 0.3999999999999993561, 0.4000000000000000777, 0.4000000000000000777, 0.3999999999999984679, 0.3999999999999984679, 0.3999999999999993561, 0.3999999999999993561),
 ( 0.3999999999999993561, 0.3999999999999993561, 0.4000000000000000777, 0.4000000000000000777, 0.4000000000000000777, 0.4000000000000000777, 0.4000000000000000777, 0.4000000000000000777, 0.3999999999999993561, 0.3999999999999993561, 0.4000000000000000777, 0.4000000000000000777, 0.3999999999999984679, 0.3999999999999984679, 0.3999999999999993561, 0.3999999999999993561),
 ( 0.5999999999999995337, 0.5999999999999995337, 0.5999999999999999778, 0.5999999999999999778, 0.5999999999999999778, 0.5999999999999999778, 0.5999999999999999778, 0.5999999999999999778, 0.5999999999999995337, 0.5999999999999995337, 0.5999999999999999778, 0.5999999999999999778, 0.5999999999999989786, 0.5999999999999989786, 0.5999999999999995337, 0.5999999999999995337),
 ( 1.000000000000000000, 1.000000000000000000, 1.000000000000000000, 1.000000000000000000, 1.000000000000000000, 1.000000000000000000, 1.000000000000000000, 1.000000000000000000, 1.000000000000000000, 1.000000000000000000, 1.000000000000000000, 1.000000000000000000, 1.000000000000000000, 1.000000000000000000, 1.000000000000000000, 1.000000000000000000) ) ) 
 REPRESENTATION_ITEM ( '' )  SURFACE ( )  );
#3233 = EDGE_CURVE ( 'NONE', #2347, #1631, #5953, .T. ) ;
#3234 = CARTESIAN_POINT ( 'NONE',  ( 18.50000000000001421, 12.50000000000001066, -1.214306433183764966E-14 ) ) ;
#3235 = ORIENTED_EDGE ( 'NONE', *, *, #5594, .T. ) ;
#3236 = CARTESIAN_POINT ( 'NONE',  ( 3.000000000000002665, -28.78532416918554304, 13.00000000000000711 ) ) ;
#3237 = LINE ( 'NONE', #5586, #552 ) ;
#3238 = APPLICATION_CONTEXT ( 'automotive_design' ) ;
#3239 = ORIENTED_EDGE ( 'NONE', *, *, #6101, .F. ) ;
#3240 = CIRCLE ( 'NONE', #6309, 13.99999999999999112 ) ;
#3241 = AXIS2_PLACEMENT_3D ( 'NONE', #4724, #2443, #2329 ) ;
#3242 = CIRCLE ( 'NONE', #6180, 15.99999999999998934 ) ;
#3243 = CARTESIAN_POINT ( 'NONE',  ( -21.49999999999999645, -219.7493155748557285, 72.39337262706533238 ) ) ;
#3244 = PLANE ( 'NONE',  #1524 ) ;
#3245 = ORIENTED_EDGE ( 'NONE', *, *, #585, .T. ) ;
#3246 = DIRECTION ( 'NONE',  ( -3.491481338843133355E-15, 1.000000000000000000, 0.000000000000000000 ) ) ;
#3247 = AXIS2_PLACEMENT_3D ( 'NONE', #1045, #5244, #4089 ) ;
#3248 = CARTESIAN_POINT ( 'NONE',  ( -53.51728042240002026, -224.0594585235269847, 96.26692417614293618 ) ) ;
#3249 = MECHANICAL_DESIGN_GEOMETRIC_PRESENTATION_REPRESENTATION (  '', ( #6566 ), #5335 ) ;
#3250 = EDGE_CURVE ( 'NONE', #1919, #5113, #5415, .T. ) ;
#3251 = CARTESIAN_POINT ( 'NONE',  ( 0.000000000000000000, 56.99999999999999289, 3.000000000000021760 ) ) ;
#3252 = EDGE_CURVE ( 'NONE', #5749, #2730, #1969, .T. ) ;
#3253 = ORIENTED_EDGE ( 'NONE', *, *, #3541, .F. ) ;
#3254 = ORIENTED_EDGE ( 'NONE', *, *, #4324, .T. ) ;
#3255 = AXIS2_PLACEMENT_3D ( 'NONE', #495, #1036, #1113 ) ;
#3256 = CIRCLE ( 'NONE', #5095, 26.99999999999999289 ) ;
#3257 = CARTESIAN_POINT ( 'NONE',  ( 0.000000000000000000, -28.78532416918554304, 10.00000000000000711 ) ) ;
#3258 = CARTESIAN_POINT ( 'NONE',  ( 47.00000000000000000, 24.90486745229362953, 37.17889356869155648 ) ) ;
#3259 = CARTESIAN_POINT ( 'NONE',  ( -21.49999999999999289, -114.1489496936987393, 42.14012972382754896 ) ) ;
#3260 = CARTESIAN_POINT ( 'NONE',  ( -62.90859119154448820, -223.0635329001938771, 78.89259148748521966 ) ) ;
#3261 = ORIENTED_EDGE ( 'NONE', *, *, #7337, .F. ) ;
#3262 = CARTESIAN_POINT ( 'NONE',  ( 188.0000000000000000, 11.00000000000000533, 0.000000000000000000 ) ) ;
#3263 = CIRCLE ( 'NONE', #678, 22.00000000000000355 ) ;
#3264 = VERTEX_POINT ( 'NONE', #1835 ) ;
#3265 = VERTEX_POINT ( 'NONE', #4193 ) ;
#3266 = VECTOR ( 'NONE', #1130, 1000.000000000000000 ) ;
#3267 = CARTESIAN_POINT ( 'NONE',  ( 220.0000000000000000, 20.99999999999999645, 13.00000000000000888 ) ) ;
#3268 = CARTESIAN_POINT ( 'NONE',  ( 13.99999999999999645, 0.000000000000000000, -39.99999999999997868 ) ) ;
#3269 = FACE_OUTER_BOUND ( 'NONE', #2995, .T. ) ;
#3270 = ORIENTED_EDGE ( 'NONE', *, *, #5828, .T. ) ;
#3271 = EDGE_CURVE ( 'NONE', #7561, #5778, #6539, .T. ) ;
#3272 = ORIENTED_EDGE ( 'NONE', *, *, #3403, .F. ) ;
#3273 = EDGE_CURVE ( 'NONE', #1595, #1663, #3036, .T. ) ;
#3274 = CIRCLE ( 'NONE', #2297, 14.00000000000000533 ) ;
#3275 = LINE ( 'NONE', #3853, #1030 ) ;
#3276 = ORIENTED_EDGE ( 'NONE', *, *, #6748, .F. ) ;
#3277 = DIRECTION ( 'NONE',  ( 1.000000000000000000, 2.624548829666596736E-30, -9.231085635203017994E-31 ) ) ;
#3278 = DIRECTION ( 'NONE',  ( 1.000000000000000000, 0.000000000000000000, 0.000000000000000000 ) ) ;
#3279 =( BOUNDED_CURVE ( )  B_SPLINE_CURVE ( 3, ( #6126, #1387, #7241, #7133 ),
 .UNSPECIFIED., .F., .T. ) 
 B_SPLINE_CURVE_WITH_KNOTS ( ( 4, 4 ),
 ( 0.000000000000000000, 1.570796326794896558 ),
 .UNSPECIFIED. ) 
 CURVE ( )  GEOMETRIC_REPRESENTATION_ITEM ( )  RATIONAL_B_SPLINE_CURVE ( ( 1.000000000000000000, 0.8047378541243649375, 0.8047378541243649375, 1.000000000000000000 ) ) 
 REPRESENTATION_ITEM ( '' )  );
#3280 = ORIENTED_EDGE ( 'NONE', *, *, #6968, .T. ) ;
#3281 = CIRCLE ( 'NONE', #5250, 5.000000000000004441 ) ;
#3282 = ADVANCED_FACE ( 'NONE', ( #2453 ), #7368, .T. ) ;
#3283 = FACE_BOUND ( 'NONE', #7249, .T. ) ;
#3284 = DIRECTION ( 'NONE',  ( -1.000000000000000000, -1.725633230170963324E-31, 1.078147950931789387E-16 ) ) ;
#3285 = CARTESIAN_POINT ( 'NONE',  ( -64.50000000000000000, -218.0630240738404950, 95.20959099461346398 ) ) ;
#3286 = ORIENTED_EDGE ( 'NONE', *, *, #1566, .F. ) ;
#3287 = AXIS2_PLACEMENT_3D ( 'NONE', #3525, #630, #15 ) ;
#3288 = CARTESIAN_POINT ( 'NONE',  ( -12.50000000000000355, -218.0630240738404382, 71.94153218116483117 ) ) ;
#3289 = CYLINDRICAL_SURFACE ( 'NONE', #5785, 9.999999999999998224 ) ;
#3290 = CARTESIAN_POINT ( 'NONE',  ( 3.000000000000002665, 60.00000000000000000, 10.00000000000002309 ) ) ;
#3291 = EDGE_LOOP ( 'NONE', ( #4164, #4593, #7086 ) ) ;
#3292 = ORIENTED_EDGE ( 'NONE', *, *, #2841, .T. ) ;
#3293 = ADVANCED_FACE ( 'NONE', ( #4340 ), #5530, .F. ) ;
#3294 = FACE_OUTER_BOUND ( 'NONE', #41, .T. ) ;
#3295 = SURFACE_STYLE_USAGE ( .BOTH. , #2824 ) ;
#3296 = CARTESIAN_POINT ( 'NONE',  ( -57.09769269110365997, -223.0630240738405803, 95.49530934758278988 ) ) ;
#3297 = DIRECTION ( 'NONE',  ( 0.000000000000000000, 0.000000000000000000, 1.000000000000000000 ) ) ;
#3298 = CARTESIAN_POINT ( 'NONE',  ( -16.30128210308657088, -115.0146905589846256, 42.92178193144403764 ) ) ;
#3299 = CARTESIAN_POINT ( 'NONE',  ( -58.92633973340381459, -218.0624722072869872, 93.67408273893140347 ) ) ;
#3300 = ORIENTED_EDGE ( 'NONE', *, *, #3787, .F. ) ;
#3301 = EDGE_CURVE ( 'NONE', #3944, #1381, #1592, .T. ) ;
#3302 = ORIENTED_EDGE ( 'NONE', *, *, #5881, .T. ) ;
#3303 = CARTESIAN_POINT ( 'NONE',  ( -21.50000000000000000, -104.1739323729103432, 75.12787131935894536 ) ) ;
#3304 = CARTESIAN_POINT ( 'NONE',  ( -53.25562355766781053, -223.0194114314942908, 73.26959217102401567 ) ) ;
#3305 = EDGE_CURVE ( 'NONE', #2919, #5270, #7335, .T. ) ;
#3306 = DIRECTION ( 'NONE',  ( 1.000000000000000000, 4.437342591868191405E-31, -3.379803290564627601E-16 ) ) ;
#3307 = CARTESIAN_POINT ( 'NONE',  ( -26.50000000000003197, -39.68629150101520509, 16.00000000000001421 ) ) ;
#3308 = ORIENTED_EDGE ( 'NONE', *, *, #2042, .T. ) ;
#3309 = ORIENTED_EDGE ( 'NONE', *, *, #3857, .F. ) ;
#3310 = CARTESIAN_POINT ( 'NONE',  ( -10.49999999999997513, -39.68629150101519087, 15.99999999999998579 ) ) ;
#3311 = ORIENTED_EDGE ( 'NONE', *, *, #3449, .F. ) ;
#3312 = ADVANCED_FACE ( 'NONE', ( #333 ), #5610, .T. ) ;
#3313 = CARTESIAN_POINT ( 'NONE',  ( 209.9999999999999716, -3.000000000000000888, 35.00000000000000000 ) ) ;
#3314 = EDGE_CURVE ( 'NONE', #5020, #5359, #4309, .T. ) ;
#3315 = CARTESIAN_POINT ( 'NONE',  ( 3.000000000000002665, 0.000000000000000000, 35.00000000000000000 ) ) ;
#3316 = EDGE_LOOP ( 'NONE', ( #1488, #5210, #1332, #4974, #509 ) ) ;
#3317 = AXIS2_PLACEMENT_3D ( 'NONE', #4992, #4260, #3760 ) ;
#3318 = FACE_OUTER_BOUND ( 'NONE', #2317, .T. ) ;
#3319 = CARTESIAN_POINT ( 'NONE',  ( -21.50000000000000000, -120.9522879036832848, 45.92078884797942351 ) ) ;
#3320 = ORIENTED_EDGE ( 'NONE', *, *, #5109, .F. ) ;
#3321 = DIRECTION ( 'NONE',  ( 7.581720952678361936E-17, -0.9999999999999997780, -1.210086977830973849E-16 ) ) ;
#3322 = EDGE_CURVE ( 'NONE', #3547, #4957, #4383, .T. ) ;
#3323 = CARTESIAN_POINT ( 'NONE',  ( -64.50000000000000000, -39.68629150101522640, 16.00000000000001421 ) ) ;
#3324 = CARTESIAN_POINT ( 'NONE',  ( 217.0000000000000000, -9.000000000000001776, 15.00000000000000888 ) ) ;
#3325 =( BOUNDED_CURVE ( )  B_SPLINE_CURVE ( 3, ( #4755, #4170, #6513, #3054 ),
 .UNSPECIFIED., .F., .T. ) 
 B_SPLINE_CURVE_WITH_KNOTS ( ( 4, 4 ),
 ( 3.141592653589793116, 4.712388980384689674 ),
 .UNSPECIFIED. ) 
 CURVE ( )  GEOMETRIC_REPRESENTATION_ITEM ( )  RATIONAL_B_SPLINE_CURVE ( ( 1.000000000000000000, 0.8047378541243649375, 0.8047378541243649375, 1.000000000000000000 ) ) 
 REPRESENTATION_ITEM ( '' )  );
#3326 = DIRECTION ( 'NONE',  ( 0.000000000000000000, 1.156482317317871725E-15, -1.000000000000000000 ) ) ;
#3327 = ORIENTED_EDGE ( 'NONE', *, *, #1317, .T. ) ;
#3328 = ORIENTED_EDGE ( 'NONE', *, *, #4523, .F. ) ;
#3329 = DIRECTION ( 'NONE',  ( 0.000000000000000000, -1.000000000000000000, -1.221245327087672392E-15 ) ) ;
#3330 = LINE ( 'NONE', #443, #5715 ) ;
#3331 = DIRECTION ( 'NONE',  ( 0.000000000000000000, 0.000000000000000000, -1.000000000000000000 ) ) ;
#3332 = CARTESIAN_POINT ( 'NONE',  ( 188.5919081759386415, 3.158066926375936223, 17.92009726762579191 ) ) ;
#3333 = EDGE_CURVE ( 'NONE', #6856, #578, #6025, .T. ) ;
#3334 = DIRECTION ( 'NONE',  ( 1.000000000000000000, 2.465190328815661892E-32, -9.244463733058732095E-33 ) ) ;
#3335 = CARTESIAN_POINT ( 'NONE',  ( -19.15685424949238325, -63.65685424949226245, 36.65685424949236193 ) ) ;
#3336 = DIRECTION ( 'NONE',  ( -2.465190328815661892E-32, -0.7071067811865465735, 0.7071067811865484609 ) ) ;
#3337 = CIRCLE ( 'NONE', #14, 3.000000000000002665 ) ;
#3338 = EDGE_CURVE ( 'NONE', #4912, #2347, #4416, .T. ) ;
#3339 = CARTESIAN_POINT ( 'NONE',  ( -57.47262553190106615, -218.0630247163618094, 72.86387756518055880 ) ) ;
#3340 = VERTEX_POINT ( 'NONE', #186 ) ;
#3341 = ORIENTED_EDGE ( 'NONE', *, *, #6156, .T. ) ;
#3342 = DIRECTION ( 'NONE',  ( -1.000000000000000000, -0.000000000000000000, -0.000000000000000000 ) ) ;
#3343 = DIRECTION ( 'NONE',  ( -2.465190328815661892E-32, -1.000000000000000000, -1.193489751472043281E-15 ) ) ;
#3344 = DIRECTION ( 'NONE',  ( -1.000000000000000000, 0.000000000000000000, 0.000000000000000000 ) ) ;
#3345 = DIRECTION ( 'NONE',  ( 0.000000000000000000, -0.1666666666666668239, -0.9860132971832694659 ) ) ;
#3346 = LINE ( 'NONE', #4079, #5807 ) ;
#3347 =( REPRESENTATION_RELATIONSHIP ('NONE','NONE', #4862, #6475 ) REPRESENTATION_RELATIONSHIP_WITH_TRANSFORMATION ( #2394 )SHAPE_REPRESENTATION_RELATIONSHIP( ) );
#3348 = EDGE_CURVE ( 'NONE', #1529, #1269, #4926, .T. ) ;
#3349 = EDGE_CURVE ( 'NONE', #920, #3850, #2101, .T. ) ;
#3350 = PRODUCT_DEFINITION ( 'UNKNOWN', '', #7315, #1175 ) ;
#3351 = ORIENTED_EDGE ( 'NONE', *, *, #2828, .T. ) ;
#3352 = ORIENTED_EDGE ( 'NONE', *, *, #4544, .F. ) ;
#3353 = VECTOR ( 'NONE', #3829, 1000.000000000000000 ) ;
#3354 = DIRECTION ( 'NONE',  ( 0.000000000000000000, 0.000000000000000000, 1.000000000000000000 ) ) ;
#3355 = EDGE_LOOP ( 'NONE', ( #784, #987, #5308, #7418 ) ) ;
#3356 = CARTESIAN_POINT ( 'NONE',  ( 188.6380400399839061, -9.000000000000001776, 15.00000000000000888 ) ) ;
#3357 = DIRECTION ( 'NONE',  ( 0.000000000000000000, 0.000000000000000000, 1.000000000000000000 ) ) ;
#3358 = ORIENTED_EDGE ( 'NONE', *, *, #4832, .F. ) ;
#3359 = CARTESIAN_POINT ( 'NONE',  ( 26.00000000000000000, 7.347880794884123680E-16, -6.000000000000003553 ) ) ;
#3360 = ORIENTED_EDGE ( 'NONE', *, *, #5531, .F. ) ;
#3361 = DIRECTION ( 'NONE',  ( -1.043412102962755161E-30, 1.000000000000000000, 1.268492242322660990E-30 ) ) ;
#3362 = CARTESIAN_POINT ( 'NONE',  ( -70.04900473833201602, -222.6575489669631054, 90.39048551345001670 ) ) ;
#3363 = FACE_OUTER_BOUND ( 'NONE', #1491, .T. ) ;
#3364 = DIRECTION ( 'NONE',  ( 9.244463733058733463E-33, 0.000000000000000000, -1.000000000000000000 ) ) ;
#3365 = VERTEX_POINT ( 'NONE', #1366 ) ;
#3366 = ORIENTED_EDGE ( 'NONE', *, *, #4384, .T. ) ;
#3367 = EDGE_CURVE ( 'NONE', #3586, #5789, #1447, .T. ) ;
#3368 = EDGE_CURVE ( 'NONE', #5318, #2966, #3690, .T. ) ;
#3369 = CARTESIAN_POINT ( 'NONE',  ( -13.64230087749234599, 16.00000000000004263, 38.63670350735201708 ) ) ;
#3370 = VECTOR ( 'NONE', #4054, 1000.000000000000000 ) ;
#3371 = VECTOR ( 'NONE', #1802, 1000.000000000000000 ) ;
#3372 = PLANE ( 'NONE',  #7183 ) ;
#3373 = CARTESIAN_POINT ( 'NONE',  ( 220.0000000000000000, 60.00000000000000000, 3.000000000000021760 ) ) ;
#3374 = DIRECTION ( 'NONE',  ( 0.000000000000000000, 0.000000000000000000, -1.000000000000000000 ) ) ;
#3375 = DIRECTION ( 'NONE',  ( 1.000000000000000000, 0.000000000000000000, 0.000000000000000000 ) ) ;
#3376 = CARTESIAN_POINT ( 'NONE',  ( -16.49999999999998934, -117.1391065123254407, 44.37576177830231217 ) ) ;
#3377 = DIRECTION ( 'NONE',  ( -0.000000000000000000, -1.000000000000000000, -3.304235192336776498E-16 ) ) ;
#3378 = CIRCLE ( 'NONE', #5472, 15.99999999999998934 ) ;
#3379 = COLOUR_RGB ( '',0.7921568627450980005, 0.8196078431372548767, 0.9333333333333333481 ) ;
#3380 = VECTOR ( 'NONE', #2305, 1000.000000000000000 ) ;
#3381 = ORIENTED_EDGE ( 'NONE', *, *, #3822, .F. ) ;
#3382 = EDGE_CURVE ( 'NONE', #584, #7026, #754, .T. ) ;
#3383 = ORIENTED_EDGE ( 'NONE', *, *, #7556, .T. ) ;
#3384 = CARTESIAN_POINT ( 'NONE',  ( -16.49999999999996447, -49.37258300203045280, -6.000000000000029310 ) ) ;
#3385 = CARTESIAN_POINT ( 'NONE',  ( 53.00000000000000711, -22.78166690339260825, 10.00000000000000711 ) ) ;
#3386 = VECTOR ( 'NONE', #1417, 1000.000000000000000 ) ;
#3387 = DIRECTION ( 'NONE',  ( -0.000000000000000000, -0.000000000000000000, 1.000000000000000000 ) ) ;
#3388 = CARTESIAN_POINT ( 'NONE',  ( 35.00000000000000000, 39.99999999999999289, 0.000000000000000000 ) ) ;
#3389 = CIRCLE ( 'NONE', #7303, 10.00000000000000178 ) ;
#3390 = CIRCLE ( 'NONE', #3133, 6.000000000000000000 ) ;
#3391 = PLANE ( 'NONE',  #2978 ) ;
#3392 = ORIENTED_EDGE ( 'NONE', *, *, #702, .T. ) ;
#3393 = PRODUCT_DEFINITION_FORMATION_WITH_SPECIFIED_SOURCE ( 'ANY', '', #6529, .NOT_KNOWN. ) ;
#3394 = EDGE_LOOP ( 'NONE', ( #4025, #4543, #3052, #3982, #1212, #5533 ) ) ;
#3395 = EDGE_CURVE ( 'NONE', #1377, #2714, #4920, .T. ) ;
#3396 = DIRECTION ( 'NONE',  ( 0.000000000000000000, 0.000000000000000000, -1.000000000000000000 ) ) ;
#3397 = ORIENTED_EDGE ( 'NONE', *, *, #6685, .T. ) ;
#3398 = CARTESIAN_POINT ( 'NONE',  ( -17.32280336819469468, -106.8228033681944993, 34.82280336819463429 ) ) ;
#3399 = DIRECTION ( 'NONE',  ( 1.000000000000000000, 0.000000000000000000, 0.000000000000000000 ) ) ;
#3400 = CARTESIAN_POINT ( 'NONE',  ( -10.49999999999997691, -45.34314575050758123, 18.34314575050765939 ) ) ;
#3401 = VERTEX_POINT ( 'NONE', #5456 ) ;
#3402 = AXIS2_PLACEMENT_3D ( 'NONE', #6958, #600, #1683 ) ;
#3403 = EDGE_CURVE ( 'NONE', #4921, #877, #1107, .T. ) ;
#3404 = FACE_OUTER_BOUND ( 'NONE', #2017, .T. ) ;
#3405 = FACE_BOUND ( 'NONE', #7158, .T. ) ;
#3406 = ORIENTED_EDGE ( 'NONE', *, *, #6395, .T. ) ;
#3407 = CARTESIAN_POINT ( 'NONE',  ( 0.000000000000000000, 0.000000000000000000, 0.000000000000000000 ) ) ;
#3408 = CARTESIAN_POINT ( 'NONE',  ( -60.72636667137881261, -216.4242598635585182, 94.92063264932016864 ) ) ;
#3409 = DIRECTION ( 'NONE',  ( -1.000000000000000000, 5.551115123125783935E-17, -4.237045877651919561E-33 ) ) ;
#3410 = LINE ( 'NONE', #3941, #6179 ) ;
#3411 = AXIS2_PLACEMENT_3D ( 'NONE', #145, #6026, #749 ) ;
#3412 = VERTEX_POINT ( 'NONE', #7221 ) ;
#3413 = PRODUCT ( 'large revit', 'large revit', '', ( #5823 ) ) ;
#3414 = ORIENTED_EDGE ( 'NONE', *, *, #5977, .F. ) ;
#3415 = VECTOR ( 'NONE', #7319, 1000.000000000000000 ) ;
#3416 = LINE ( 'NONE', #6863, #5619 ) ;
#3417 = SURFACE_STYLE_USAGE ( .BOTH. , #1509 ) ;
#3418 = DIRECTION ( 'NONE',  ( -1.000000000000000000, 5.551115123125783935E-17, -4.237045877651919561E-33 ) ) ;
#3419 = CARTESIAN_POINT ( 'NONE',  ( 217.0000000000000000, 56.99999999999999289, 3.000000000000021760 ) ) ;
#3420 = CARTESIAN_POINT ( 'NONE',  ( 10.25759302228802738, -223.0630240738404382, 73.28127814332047762 ) ) ;
#3421 = LINE ( 'NONE', #2830, #1586 ) ;
#3422 = EDGE_CURVE ( 'NONE', #868, #1940, #829, .T. ) ;
#3423 = CARTESIAN_POINT ( 'NONE',  ( -58.07354361304951595, -218.0631760585727932, 73.14332378351642205 ) ) ;
#3424 = AXIS2_PLACEMENT_3D ( 'NONE', #2345, #81, #1762 ) ;
#3425 = UNCERTAINTY_MEASURE_WITH_UNIT (LENGTH_MEASURE( 1.000000000000000082E-05 ), #632, 'distance_accuracy_value', 'NONE');
#3426 = ORIENTED_EDGE ( 'NONE', *, *, #1670, .F. ) ;
#3427 = EDGE_LOOP ( 'NONE', ( #7486, #5862, #5851 ) ) ;
#3428 = DIRECTION ( 'NONE',  ( 0.000000000000000000, 1.000000000000000000, 0.000000000000000000 ) ) ;
#3429 = CARTESIAN_POINT ( 'NONE',  ( 0.000000000000000000, 30.03170604878415162, 7.000000000000013323 ) ) ;
#3430 = FACE_OUTER_BOUND ( 'NONE', #168, .T. ) ;
#3431 = CARTESIAN_POINT ( 'NONE',  ( -21.50000000000000000, -99.90626354475340065, 72.90626354475362803 ) ) ;
#3432 = ORIENTED_EDGE ( 'NONE', *, *, #2363, .T. ) ;
#3433 = ORIENTED_EDGE ( 'NONE', *, *, #2439, .T. ) ;
#3434 = DIRECTION ( 'NONE',  ( 4.336808689942025132E-16, 2.255140518769853009E-14, 1.000000000000000000 ) ) ;
#3435 = DIRECTION ( 'NONE',  ( -1.000000000000000000, -0.000000000000000000, 0.000000000000000000 ) ) ;
#3436 = EDGE_LOOP ( 'NONE', ( #1384, #4582, #3426, #7042 ) ) ;
#3437 = CARTESIAN_POINT ( 'NONE',  ( -16.49999999999996447, -102.6862915010150203, 30.68629150101515179 ) ) ;
#3438 = FACE_OUTER_BOUND ( 'NONE', #5251, .T. ) ;
#3439 = EDGE_CURVE ( 'NONE', #5727, #2116, #864, .T. ) ;
#3440 = ORIENTED_EDGE ( 'NONE', *, *, #7397, .F. ) ;
#3441 = DIRECTION ( 'NONE',  ( -1.000000000000000000, -1.725633230170963324E-31, 1.078147950931789387E-16 ) ) ;
#3442 = CARTESIAN_POINT ( 'NONE',  ( 17.76462208873361348, -219.0153713307822727, 95.37751551101582947 ) ) ;
#3443 = ORIENTED_EDGE ( 'NONE', *, *, #6405, .T. ) ;
#3444 = CARTESIAN_POINT ( 'NONE',  ( 200.0000000000000000, 0.000000000000000000, 14.00000000000000533 ) ) ;
#3445 = CARTESIAN_POINT ( 'NONE',  ( -26.52830334398518985, -116.3958977277557807, 43.92260702357706492 ) ) ;
#3446 = ORIENTED_EDGE ( 'NONE', *, *, #2139, .T. ) ;
#3447 = EDGE_CURVE ( 'NONE', #5693, #4453, #2641, .T. ) ;
#3448 = VERTEX_POINT ( 'NONE', #2792 ) ;
#3449 = EDGE_CURVE ( 'NONE', #5895, #7386, #361, .T. ) ;
#3450 = DIRECTION ( 'NONE',  ( 1.000000000000000000, -0.000000000000000000, -0.000000000000000000 ) ) ;
#3451 = CLOSED_SHELL ( 'NONE', ( #465, #6068, #4341, #7279, #6235, #515, #5086, #6426, #7290, #7328, #689, #7017, #7004, #6664 ) ) ;
#3452 = CARTESIAN_POINT ( 'NONE',  ( 0.000000000000000000, 0.000000000000000000, -9.999999999999994671 ) ) ;
#3453 = AXIS2_PLACEMENT_3D ( 'NONE', #7402, #1555, #2136 ) ;
#3454 = CARTESIAN_POINT ( 'NONE',  ( 191.6458868871019661, 6.000000000000000888, 17.60487178029247346 ) ) ;
#3455 = CARTESIAN_POINT ( 'NONE',  ( 20.57205124765284765, -218.0630240738404950, 88.30031236728251542 ) ) ;
#3456 = CARTESIAN_POINT ( 'NONE',  ( 13.34421828821804112, -223.0630240738404950, 73.71416242504422200 ) ) ;
#3457 = CARTESIAN_POINT ( 'NONE',  ( 47.00000000000000000, 27.28271252673189196, 10.00000000000001421 ) ) ;
#3458 = CARTESIAN_POINT ( 'NONE',  ( -63.83888562197329009, -218.0637078869157506, 79.76758675555454658 ) ) ;
#3459 = ORIENTED_EDGE ( 'NONE', *, *, #2992, .F. ) ;
#3460 = DIRECTION ( 'NONE',  ( 0.000000000000000000, 0.000000000000000000, 1.000000000000000000 ) ) ;
#3461 = DIRECTION ( 'NONE',  ( -1.000000000000000000, 5.551115123125783935E-17, -4.237045877651919561E-33 ) ) ;
#3462 = CARTESIAN_POINT ( 'NONE',  ( -13.49999999999999822, -223.0630240738404666, 96.09122589815579829 ) ) ;
#3463 = AXIS2_PLACEMENT_3D ( 'NONE', #3674, #735, #4283 ) ;
#3464 = CARTESIAN_POINT ( 'NONE',  ( -26.50000000000003197, -49.37258300203047412, 0.000000000000000000 ) ) ;
#3465 = VERTEX_POINT ( 'NONE', #4033 ) ;
#3466 = VERTEX_POINT ( 'NONE', #5108 ) ;
#3467 = DIRECTION ( 'NONE',  ( 1.000000000000000000, 2.465190328815661892E-32, -9.244463733058732095E-33 ) ) ;
#3468 = LINE ( 'NONE', #2313, #4610 ) ;
#3469 = CARTESIAN_POINT ( 'NONE',  ( -18.84314575050759188, -108.3431457505073752, 36.34314575050756702 ) ) ;
#3470 = CARTESIAN_POINT ( 'NONE',  ( 3.000000000000002665, -24.98477067547739239, 35.87248741756260983 ) ) ;
#3471 = EDGE_LOOP ( 'NONE', ( #1260, #6182, #1909 ) ) ;
#3472 = AXIS2_PLACEMENT_3D ( 'NONE', #2108, #3228, #4963 ) ;
#3473 = ORIENTED_EDGE ( 'NONE', *, *, #7228, .T. ) ;
#3474 = ADVANCED_FACE ( 'NONE', ( #1514 ), #3878, .T. ) ;
#3475 = CARTESIAN_POINT ( 'NONE',  ( 17.99999999999999645, 0.000000000000000000, -9.999999999999994671 ) ) ;
#3476 = CARTESIAN_POINT ( 'NONE',  ( 27.12218822116579631, -219.3688186872617223, 89.73635190582673715 ) ) ;
#3477 = VERTEX_POINT ( 'NONE', #1095 ) ;
#3478 = SHAPE_DEFINITION_REPRESENTATION ( #3534, #2538 ) ;
#3479 = DIRECTION ( 'NONE',  ( 0.000000000000000000, 1.000000000000000000, -0.000000000000000000 ) ) ;
#3480 = CARTESIAN_POINT ( 'NONE',  ( 12.50000000000000355, 101.5000000000000000, -1.214306433183764966E-14 ) ) ;
#3481 = EDGE_LOOP ( 'NONE', ( #1051, #7570, #384, #955 ) ) ;
#3482 = FACE_OUTER_BOUND ( 'NONE', #6244, .T. ) ;
#3483 = EDGE_CURVE ( 'NONE', #1377, #5154, #6999, .T. ) ;
#3484 = DIRECTION ( 'NONE',  ( 5.605193857299270773E-45, 0.000000000000000000, 1.000000000000000000 ) ) ;
#3485 = ADVANCED_FACE ( 'NONE', ( #403, #448 ), #5760, .F. ) ;
#3486 =( NAMED_UNIT ( * ) PLANE_ANGLE_UNIT ( ) SI_UNIT ( $, .RADIAN. ) );
#3487 = CARTESIAN_POINT ( 'NONE',  ( 15.34038085515988392, -218.0630240738405519, 93.99974598701426487 ) ) ;
#3488 = CARTESIAN_POINT ( 'NONE',  ( -26.50000000000003197, -102.6862915010150346, 30.68629150101517666 ) ) ;
#3489 = PRODUCT_DEFINITION_SHAPE ( 'NONE', 'NONE',  #7607 ) ;
#3490 = UNCERTAINTY_MEASURE_WITH_UNIT (LENGTH_MEASURE( 1.000000000000000082E-05 ), #743, 'distance_accuracy_value', 'NONE');
#3491 = CIRCLE ( 'NONE', #3616, 3.000000000000000888 ) ;
#3492 = VERTEX_POINT ( 'NONE', #5680 ) ;
#3493 = EDGE_CURVE ( 'NONE', #6371, #3543, #4607, .T. ) ;
#3494 = SURFACE_STYLE_USAGE ( .BOTH. , #1136 ) ;
#3495 = DIRECTION ( 'NONE',  ( 0.000000000000000000, 0.000000000000000000, -1.000000000000000000 ) ) ;
#3496 = DIRECTION ( 'NONE',  ( 0.000000000000000000, 0.000000000000000000, -1.000000000000000000 ) ) ;
#3497 = LINE ( 'NONE', #4192, #4354 ) ;
#3498 = DIRECTION ( 'NONE',  ( 1.000000000000000000, 2.465190328815661892E-32, -9.244463733058732095E-33 ) ) ;
#3499 = AXIS2_PLACEMENT_3D ( 'NONE', #46, #1312, #660 ) ;
#3500 = CIRCLE ( 'NONE', #4736, 7.000000000000017764 ) ;
#3501 = AXIS2_PLACEMENT_3D ( 'NONE', #3922, #2147, #4973 ) ;
#3502 = ORIENTED_EDGE ( 'NONE', *, *, #9, .F. ) ;
#3503 = VERTEX_POINT ( 'NONE', #2180 ) ;
#3504 = CIRCLE ( 'NONE', #4241, 8.500000000000007105 ) ;
#3505 = VECTOR ( 'NONE', #2328, 1000.000000000000227 ) ;
#3506 = CARTESIAN_POINT ( 'NONE',  ( -26.50000000000003197, 0.000000000000000000, 0.000000000000000000 ) ) ;
#3507 = CARTESIAN_POINT ( 'NONE',  ( -29.64230087749236731, -65.39789427971169289, 38.39789427971179947 ) ) ;
#3508 = ORIENTED_EDGE ( 'NONE', *, *, #984, .F. ) ;
#3509 = CARTESIAN_POINT ( 'NONE',  ( 37.99999999999998579, -4.040871662429601878E-14, -9.999999999999984013 ) ) ;
#3510 = DIRECTION ( 'NONE',  ( -1.681558157189779738E-44, 0.000000000000000000, -1.000000000000000000 ) ) ;
#3511 = ADVANCED_FACE ( 'NONE', ( #7519 ), #5798, .F. ) ;
#3512 = CIRCLE ( 'NONE', #7414, 13.99999999999999645 ) ;
#3513 = AXIS2_PLACEMENT_3D ( 'NONE', #2337, #7030, #1756 ) ;
#3514 = EDGE_CURVE ( 'NONE', #1226, #1572, #4679, .T. ) ;
#3515 = VERTEX_POINT ( 'NONE', #4534 ) ;
#3516 = ORIENTED_EDGE ( 'NONE', *, *, #5438, .T. ) ;
#3517 = LINE ( 'NONE', #432, #2998 ) ;
#3518 = CARTESIAN_POINT ( 'NONE',  ( 17.77671317003690632, -219.8343230396697550, 95.52191879319198620 ) ) ;
#3519 = ORIENTED_EDGE ( 'NONE', *, *, #3019, .F. ) ;
#3520 = APPLICATION_PROTOCOL_DEFINITION ( 'draft international standard', 'automotive_design', 1998, #2555 ) ;
#3521 = CARTESIAN_POINT ( 'NONE',  ( -21.50000000000000000, -114.3401965514817817, 42.31370849898471675 ) ) ;
#3522 = DIRECTION ( 'NONE',  ( 0.000000000000000000, 0.000000000000000000, -1.000000000000000000 ) ) ;
#3523 = EDGE_CURVE ( 'NONE', #2172, #2464, #2067, .T. ) ;
#3524 = VERTEX_POINT ( 'NONE', #5064 ) ;
#3525 = CARTESIAN_POINT ( 'NONE',  ( -8.500000000000003553, 16.00000000000003908, 44.76505905230376925 ) ) ;
#3526 = AXIS2_PLACEMENT_3D ( 'NONE', #2106, #6141, #5574 ) ;
#3527 = SHAPE_REPRESENTATION_RELATIONSHIP ( 'NONE' , 'NONE' ,  #915, #4741 ) ;
#3528 = DIRECTION ( 'NONE',  ( 0.000000000000000000, 0.000000000000000000, 1.000000000000000000 ) ) ;
#3529 = CARTESIAN_POINT ( 'NONE',  ( -64.50000000000000000, -99.90626354475342907, 72.90626354475362803 ) ) ;
#3530 = FACE_OUTER_BOUND ( 'NONE', #4454, .T. ) ;
#3531 = ADVANCED_FACE ( 'NONE', ( #7447 ), #366, .T. ) ;
#3532 = ORIENTED_EDGE ( 'NONE', *, *, #3931, .T. ) ;
#3533 = EDGE_LOOP ( 'NONE', ( #7260, #6874, #5584, #3627, #3308, #3765, #1999 ) ) ;
#3534 = PRODUCT_DEFINITION_SHAPE ( 'NONE', 'NONE',  #6635 ) ;
#3535 = CARTESIAN_POINT ( 'NONE',  ( 187.5739056480075533, -3.719611233821797480, 16.15686516701557807 ) ) ;
#3536 = CARTESIAN_POINT ( 'NONE',  ( 217.0000000000000000, -15.08392021690038121, 12.00000000000000711 ) ) ;
#3537 = DIRECTION ( 'NONE',  ( 0.000000000000000000, -1.000000000000000000, 0.000000000000000000 ) ) ;
#3538 = DIRECTION ( 'NONE',  ( 5.605193857299270773E-45, 0.000000000000000000, 1.000000000000000000 ) ) ;
#3539 = DIRECTION ( 'NONE',  ( -1.000000000000000000, -2.624548829666596736E-30, 9.231085635203017994E-31 ) ) ;
#3540 = AXIS2_PLACEMENT_3D ( 'NONE', #4028, #4098, #2255 ) ;
#3541 = EDGE_CURVE ( 'NONE', #3477, #2174, #980, .T. ) ;
#3542 = ORIENTED_EDGE ( 'NONE', *, *, #3673, .T. ) ;
#3543 = VERTEX_POINT ( 'NONE', #2220 ) ;
#3544 = EDGE_CURVE ( 'NONE', #4795, #3854, #480, .T. ) ;
#3545 = FACE_BOUND ( 'NONE', #2274, .T. ) ;
#3546 = CARTESIAN_POINT ( 'NONE',  ( -53.47314606205194565, -223.0630240738404950, 96.09122589815579829 ) ) ;
#3547 = VERTEX_POINT ( 'NONE', #6292 ) ;
#3548 = CARTESIAN_POINT ( 'NONE',  ( -60.70193531918452123, -219.7017882839737695, 72.38063772785841365 ) ) ;
#3549 = LINE ( 'NONE', #3082, #7504 ) ;
#3550 = DIRECTION ( 'NONE',  ( 5.551115123125783935E-17, 1.000000000000000000, -2.214819436045321778E-32 ) ) ;
#3551 = ORIENTED_EDGE ( 'NONE', *, *, #6933, .F. ) ;
#3552 = ORIENTED_EDGE ( 'NONE', *, *, #984, .T. ) ;
#3553 = EDGE_CURVE ( 'NONE', #6174, #2578, #489, .T. ) ;
#3554 = DIRECTION ( 'NONE',  ( 1.000000000000000000, 2.624548829666596736E-30, -9.231085635203017994E-31 ) ) ;
#3555 = CARTESIAN_POINT ( 'NONE',  ( 0.000000000000000000, 0.000000000000000000, 4.999999999999999112 ) ) ;
#3556 = ORIENTED_EDGE ( 'NONE', *, *, #3575, .F. ) ;
#3557 = APPLICATION_PROTOCOL_DEFINITION ( 'draft international standard', 'automotive_design', 1998, #3238 ) ;
#3558 = DIRECTION ( 'NONE',  ( -1.000000000000000000, 0.000000000000000000, 0.000000000000000000 ) ) ;
#3559 = CARTESIAN_POINT ( 'NONE',  ( 47.00000000000000000, 0.000000000000000000, 60.00000000000000711 ) ) ;
#3560 = VERTEX_POINT ( 'NONE', #1059 ) ;
#3561 = DIRECTION ( 'NONE',  ( 0.8660254037844400399, 0.000000000000000000, -0.4999999999999976685 ) ) ;
#3562 = CARTESIAN_POINT ( 'NONE',  ( 0.000000000000000000, 0.000000000000000000, 0.000000000000000000 ) ) ;
#3563 = CARTESIAN_POINT ( 'NONE',  ( 53.00000000000000000, 27.53693130344647955, 10.00000000000001066 ) ) ;
#3564 = CARTESIAN_POINT ( 'NONE',  ( 20.30051329250314396, -218.0630240738406087, 78.41711159333182479 ) ) ;
#3565 = CARTESIAN_POINT ( 'NONE',  ( 15.45545259347109379, -223.0630240738404950, 94.88225035920650896 ) ) ;
#3566 = CARTESIAN_POINT ( 'NONE',  ( -10.49999999999996803, -49.37258300203047412, -15.99999999999998579 ) ) ;
#3567 = ORIENTED_EDGE ( 'NONE', *, *, #1061, .T. ) ;
#3568=STYLED_ITEM('',(#7631),#3747);
#3569 = PLANE ( 'NONE',  #1929 ) ;
#3570 = EDGE_CURVE ( 'NONE', #2284, #3944, #3421, .T. ) ;
#3571 = SURFACE_STYLE_USAGE ( .BOTH. , #4773 ) ;
#3572 = DIRECTION ( 'NONE',  ( 0.000000000000000000, 1.000000000000000000, 2.065146995210484941E-16 ) ) ;
#3573 = CARTESIAN_POINT ( 'NONE',  ( -11.51602904742826716, -63.85254959896234794, 36.85254959896245452 ) ) ;
#3574 = CARTESIAN_POINT ( 'NONE',  ( 4.000000000000003553, 7.347880794884120722E-16, -5.999999999999986677 ) ) ;
#3575 = EDGE_CURVE ( 'NONE', #3524, #5445, #1993, .T. ) ;
#3576 = CARTESIAN_POINT ( 'NONE',  ( 36.00000000000000000, 0.000000000000000000, 1.387778780781445676E-14 ) ) ;
#3577 = VECTOR ( 'NONE', #6106, 1000.000000000000000 ) ;
#3578 =( BOUNDED_CURVE ( )  B_SPLINE_CURVE ( 3, ( #6657, #1379, #3742, #6083 ),
 .UNSPECIFIED., .F., .T. ) 
 B_SPLINE_CURVE_WITH_KNOTS ( ( 4, 4 ),
 ( 0.7853981633974504994, 1.570796326794896558 ),
 .UNSPECIFIED. ) 
 CURVE ( )  GEOMETRIC_REPRESENTATION_ITEM ( )  RATIONAL_B_SPLINE_CURVE ( ( 1.000000000000000000, 0.9492530216741914550, 0.9492530216741914550, 1.000000000000000000 ) ) 
 REPRESENTATION_ITEM ( '' )  );
#3579 = VERTEX_POINT ( 'NONE', #6490 ) ;
#3580 = ORIENTED_EDGE ( 'NONE', *, *, #3514, .F. ) ;
#3581 = VECTOR ( 'NONE', #2169, 1000.000000000000000 ) ;
#3582 = CARTESIAN_POINT ( 'NONE',  ( 26.49999999999999645, -39.99999999999999289, 10.00000000000000355 ) ) ;
#3583 = CARTESIAN_POINT ( 'NONE',  ( -13.99999999999999645, 1.714505518806293652E-15, -39.99999999999997868 ) ) ;
#3584 = ADVANCED_FACE ( 'NONE', ( #2445 ), #7103, .T. ) ;
#3585 = EDGE_CURVE ( 'NONE', #6764, #6974, #1174, .T. ) ;
#3586 = VERTEX_POINT ( 'NONE', #3566 ) ;
#3587 = CARTESIAN_POINT ( 'NONE',  ( -70.25616595088855831, -215.8398321358105818, 77.29937933778069237 ) ) ;
#3588 = CARTESIAN_POINT ( 'NONE',  ( 47.39276988301253368, -25.78715168812822611, 12.89530150989326707 ) ) ;
#3589 = DIRECTION ( 'NONE',  ( 0.000000000000000000, 0.000000000000000000, -1.000000000000000000 ) ) ;
#3590 = PRODUCT_DEFINITION ( 'UNKNOWN', '', #2034, #4187 ) ;
#3591 = AXIS2_PLACEMENT_3D ( 'NONE', #5741, #6270, #5855 ) ;
#3592 = ORIENTED_EDGE ( 'NONE', *, *, #1642, .T. ) ;
#3593 = ORIENTED_EDGE ( 'NONE', *, *, #7127, .F. ) ;
#3594 = DIRECTION ( 'NONE',  ( 1.000000000000000000, 0.000000000000000000, 0.000000000000000000 ) ) ;
#3595 = CARTESIAN_POINT ( 'NONE',  ( 9.987668098222851398, -212.1022451272886826, 94.15854484029739524 ) ) ;
#3596 = ORIENTED_EDGE ( 'NONE', *, *, #2800, .F. ) ;
#3597 = DIRECTION ( 'NONE',  ( 0.000000000000000000, 0.000000000000000000, 1.000000000000000000 ) ) ;
#3598 = DIRECTION ( 'NONE',  ( -7.006492321624086910E-46, 1.221245327087672392E-15, -1.000000000000000000 ) ) ;
#3599 = CIRCLE ( 'NONE', #6295, 8.500000000000007105 ) ;
#3600 = ORIENTED_EDGE ( 'NONE', *, *, #1954, .T. ) ;
#3601 = DIRECTION ( 'NONE',  ( 0.000000000000000000, -0.9993908270190955401, 0.03489949670250346025 ) ) ;
#3602 = CYLINDRICAL_SURFACE ( 'NONE', #5350, 4.999999999999999112 ) ;
#3603 = CARTESIAN_POINT ( 'NONE',  ( 25.00000000000001421, 80.85786437626907741, 8.071067811865434649 ) ) ;
#3604 = CARTESIAN_POINT ( 'NONE',  ( 20.41805204809246632, -218.0630240738405234, 88.64886852284689667 ) ) ;
#3605 = CARTESIAN_POINT ( 'NONE',  ( 0.000000000000000000, 0.000000000000000000, -39.99999999999997868 ) ) ;
#3606 = DIRECTION ( 'NONE',  ( 0.000000000000000000, -1.000000000000000000, -3.304235192336776498E-16 ) ) ;
#3607 = ADVANCED_FACE ( 'NONE', ( #3530 ), #635, .T. ) ;
#3608 = EDGE_CURVE ( 'NONE', #877, #4921, #1099, .T. ) ;
#3609 = CARTESIAN_POINT ( 'NONE',  ( 21.50000000000000000, -113.7796841263388501, 41.77968412633906325 ) ) ;
#3610 = CYLINDRICAL_SURFACE ( 'NONE', #5093, 9.999999999999998224 ) ;
#3611 = CYLINDRICAL_SURFACE ( 'NONE', #23, 3.000000000000002665 ) ;
#3612 = DIRECTION ( 'NONE',  ( -1.000000000000000000, 0.000000000000000000, 0.000000000000000000 ) ) ;
#3613 = DIRECTION ( 'NONE',  ( 0.000000000000000000, 0.000000000000000000, -1.000000000000000000 ) ) ;
#3614 = CARTESIAN_POINT ( 'NONE',  ( 191.6486100594302684, -6.000000000000000888, 17.60723011670769722 ) ) ;
#3615 = ADVANCED_FACE ( 'NONE', ( #6413 ), #5781, .T. ) ;
#3616 = AXIS2_PLACEMENT_3D ( 'NONE', #2415, #4111, #6461 ) ;
#3617 = VERTEX_POINT ( 'NONE', #1250 ) ;
#3618 = PRODUCT_DEFINITION_SHAPE ( 'NONE', 'NONE',  #7609 ) ;
#3619 = ORIENTED_EDGE ( 'NONE', *, *, #6866, .F. ) ;
#3620 = CYLINDRICAL_SURFACE ( 'NONE', #814, 9.999999999999996447 ) ;
#3621 = DIRECTION ( 'NONE',  ( 0.000000000000000000, 0.000000000000000000, 1.000000000000000000 ) ) ;
#3622 = AXIS2_PLACEMENT_3D ( 'NONE', #7068, #5911, #5949 ) ;
#3623 = ORIENTED_EDGE ( 'NONE', *, *, #5632, .F. ) ;
#3624 = CARTESIAN_POINT ( 'NONE',  ( -70.10306686690893230, -222.6535482193572477, 78.96676008164921257 ) ) ;
#3625 = PRESENTATION_STYLE_ASSIGNMENT (( #1846 ) ) ;
#3626 = CARTESIAN_POINT ( 'NONE',  ( -64.50000000000000000, 0.000000000000000000, 15.99999999999998579 ) ) ;
#3627 = ORIENTED_EDGE ( 'NONE', *, *, #6450, .T. ) ;
#3628 = CIRCLE ( 'NONE', #187, 5.000000000000004441 ) ;
#3629 = VECTOR ( 'NONE', #2214, 1000.000000000000000 ) ;
#3630 = EDGE_CURVE ( 'NONE', #6935, #6160, #2216, .T. ) ;
#3631 = TOROIDAL_SURFACE ( 'NONE', #4243, 24.00000000000000000, 3.000000000000000000 ) ;
#3632 = ORIENTED_EDGE ( 'NONE', *, *, #6304, .T. ) ;
#3633 = LINE ( 'NONE', #5932, #3125 ) ;
#3634 = DIRECTION ( 'NONE',  ( 1.000000000000000000, 2.465190328815661892E-32, -9.244463733058732095E-33 ) ) ;
#3635 = AXIS2_PLACEMENT_3D ( 'NONE', #4619, #3345, #5648 ) ;
#3636 = AXIS2_PLACEMENT_3D ( 'NONE', #536, #2280, #6471 ) ;
#3637 = CARTESIAN_POINT ( 'NONE',  ( -16.50000000000000000, -214.0630240738404382, 70.86973541144034527 ) ) ;
#3638 = AXIS2_PLACEMENT_3D ( 'NONE', #5061, #3913, #5719 ) ;
#3639 = ORIENTED_EDGE ( 'NONE', *, *, #3514, .T. ) ;
#3640 = EDGE_CURVE ( 'NONE', #7269, #2056, #6563, .T. ) ;
#3641 = EDGE_CURVE ( 'NONE', #5055, #2919, #626, .T. ) ;
#3642 = CARTESIAN_POINT ( 'NONE',  ( 25.00000000000000000, 12.49999999999998401, 0.000000000000000000 ) ) ;
#3643 = CYLINDRICAL_SURFACE ( 'NONE', #6323, 6.000000000000000000 ) ;
#3644 = APPLICATION_CONTEXT ( 'automotive_design' ) ;
#3645 = DIRECTION ( 'NONE',  ( 5.551115123125783935E-17, 0.7071067811865499042, 0.7071067811865451302 ) ) ;
#3646 = DIRECTION ( 'NONE',  ( 0.000000000000000000, 0.000000000000000000, 1.000000000000000000 ) ) ;
#3647 = DIRECTION ( 'NONE',  ( 1.000000000000000000, 0.000000000000000000, 0.000000000000000000 ) ) ;
#3648 = CARTESIAN_POINT ( 'NONE',  ( 53.00000000000000711, 20.99999999999999645, 10.00000000000001066 ) ) ;
#3649 = EDGE_LOOP ( 'NONE', ( #268, #3406, #6234, #3063 ) ) ;
#3650 = CIRCLE ( 'NONE', #567, 25.00000000000000000 ) ;
#3651 = DIRECTION ( 'NONE',  ( 0.000000000000000000, 0.000000000000000000, 1.000000000000000000 ) ) ;
#3652 = CARTESIAN_POINT ( 'NONE',  ( 49.73397419454932589, 25.59482593276749895, 10.00000000000000178 ) ) ;
#3653 = DIRECTION ( 'NONE',  ( 1.000000000000000000, 0.000000000000000000, 0.000000000000000000 ) ) ;
#3654 = DIRECTION ( 'NONE',  ( 1.224646799147352714E-16, 1.000000000000000000, -6.864382715941954980E-61 ) ) ;
#3655 = EDGE_CURVE ( 'NONE', #472, #2722, #5874, .T. ) ;
#3656 = LINE ( 'NONE', #6498, #1022 ) ;
#3657 = CARTESIAN_POINT ( 'NONE',  ( 187.2689031676866307, -7.021191553082208436, 15.62858537466729025 ) ) ;
#3658 = AXIS2_PLACEMENT_3D ( 'NONE', #4771, #4839, #5452 ) ;
#3659 = ORIENTED_EDGE ( 'NONE', *, *, #5209, .F. ) ;
#3660 = EDGE_LOOP ( 'NONE', ( #3805, #994, #491, #2859 ) ) ;
#3661 = DIRECTION ( 'NONE',  ( 5.551115123125783935E-17, 1.000000000000000000, 5.166928274020107347E-17 ) ) ;
#3662 = CIRCLE ( 'NONE', #334, 3.000000000000000000 ) ;
#3663 = DIRECTION ( 'NONE',  ( -1.000000000000000000, 0.000000000000000000, 0.000000000000000000 ) ) ;
#3664 = PRODUCT_DEFINITION_SHAPE ( 'NONE', 'NONE',  #7601 ) ;
#3665 = CARTESIAN_POINT ( 'NONE',  ( -53.01709100512437089, -217.7372475398855443, 71.85424062197864714 ) ) ;
#3666 = DIRECTION ( 'NONE',  ( 3.379803290564627601E-16, -1.193489751472043281E-15, 1.000000000000000000 ) ) ;
#3667 = CARTESIAN_POINT ( 'NONE',  ( -63.70446932513453220, -218.0630240022875910, 87.95745700536116374 ) ) ;
#3668 = ORIENTED_EDGE ( 'NONE', *, *, #702, .F. ) ;
#3669 = ORIENTED_EDGE ( 'NONE', *, *, #831, .T. ) ;
#3670 = FACE_OUTER_BOUND ( 'NONE', #6296, .T. ) ;
#3671 = CARTESIAN_POINT ( 'NONE',  ( 10.29386626619291434, -223.8662738488881701, 73.49650827186496826 ) ) ;
#3672 = ORIENTED_EDGE ( 'NONE', *, *, #6864, .T. ) ;
#3673 = EDGE_CURVE ( 'NONE', #551, #7269, #2490, .T. ) ;
#3674 = CARTESIAN_POINT ( 'NONE',  ( 50.00000000000000000, 0.000000000000000000, 35.00000000000000000 ) ) ;
#3675 = DIRECTION ( 'NONE',  ( -2.465190328815661892E-32, -1.000000000000000000, -1.193489751472043281E-15 ) ) ;
#3676 = ORIENTED_EDGE ( 'NONE', *, *, #5864, .F. ) ;
#3677 = LINE ( 'NONE', #5982, #5744 ) ;
#3678 = CARTESIAN_POINT ( 'NONE',  ( 217.0000000000000000, -56.99999999999999289, 3.000000000000000000 ) ) ;
#3679 = ORIENTED_EDGE ( 'NONE', *, *, #7167, .T. ) ;
#3680 = FACE_OUTER_BOUND ( 'NONE', #1516, .T. ) ;
#3681 = EDGE_CURVE ( 'NONE', #589, #2111, #5837, .T. ) ;
#3682 = DIRECTION ( 'NONE',  ( 0.000000000000000000, 0.000000000000000000, -1.000000000000000000 ) ) ;
#3683 = DIRECTION ( 'NONE',  ( -4.622231866529368100E-33, 2.600005424922769496E-32, -1.000000000000000000 ) ) ;
#3684 = ORIENTED_EDGE ( 'NONE', *, *, #5076, .F. ) ;
#3685 = CARTESIAN_POINT ( 'NONE',  ( -21.50000000000000000, -99.90626354475340065, 72.90626354475362803 ) ) ;
#3686 = SURFACE_SIDE_STYLE ('',( #4914 ) ) ;
#3687 = CARTESIAN_POINT ( 'NONE',  ( 40.00000000000000000, -4.053118130421075393E-14, -7.999999999999972466 ) ) ;
#3688 = LINE ( 'NONE', #3217, #5597 ) ;
#3689 = DIRECTION ( 'NONE',  ( -4.336808689942013792E-16, 0.000000000000000000, 1.000000000000000000 ) ) ;
#3690 = LINE ( 'NONE', #3803, #6883 ) ;
#3691 = AXIS2_PLACEMENT_3D ( 'NONE', #1676, #6952, #6377 ) ;
#3692 = ORIENTED_EDGE ( 'NONE', *, *, #1410, .T. ) ;
#3693 = EDGE_LOOP ( 'NONE', ( #2041, #7579, #6400, #1850 ) ) ;
#3694 = DIRECTION ( 'NONE',  ( 9.244463733058733463E-33, 0.000000000000000000, -1.000000000000000000 ) ) ;
#3695 = CARTESIAN_POINT ( 'NONE',  ( 30.00000000000000000, 0.000000000000000000, 0.000000000000000000 ) ) ;
#3696 = VECTOR ( 'NONE', #7518, 1000.000000000000000 ) ;
#3697 = AXIS2_PLACEMENT_3D ( 'NONE', #684, #2416, #4776 ) ;
#3698 = CARTESIAN_POINT ( 'NONE',  ( -70.12317295347672541, -219.3245666396718718, 89.72755010419726318 ) ) ;
#3699 = CARTESIAN_POINT ( 'NONE',  ( 48.55648163125127326, -25.48496883304055061, 10.00000000000205169 ) ) ;
#3700 = CARTESIAN_POINT ( 'NONE',  ( -64.49624945276272570, -218.0628238658616738, 84.01119032334271708 ) ) ;
#3701 = EDGE_LOOP ( 'NONE', ( #2653, #5014, #7487, #6306 ) ) ;
#3702 = EDGE_CURVE ( 'NONE', #5020, #7224, #1711, .T. ) ;
#3703 = ORIENTED_EDGE ( 'NONE', *, *, #3797, .F. ) ;
#3704 = FACE_OUTER_BOUND ( 'NONE', #4105, .T. ) ;
#3705 = PLANE ( 'NONE',  #7184 ) ;
#3706 = ORIENTED_EDGE ( 'NONE', *, *, #3201, .T. ) ;
#3707 = TOROIDAL_SURFACE ( 'NONE', #6407, 24.00000000000000000, 3.000000000000000000 ) ;
#3708 = DIRECTION ( 'NONE',  ( 1.000000000000000000, 2.624548829666596736E-30, -9.231085635203017994E-31 ) ) ;
#3709 = FACE_OUTER_BOUND ( 'NONE', #654, .T. ) ;
#3710 = ORIENTED_EDGE ( 'NONE', *, *, #4429, .F. ) ;
#3711 = EDGE_CURVE ( 'NONE', #105, #5964, #7008, .T. ) ;
#3712 = CARTESIAN_POINT ( 'NONE',  ( 36.00000000000000000, -4.040871662429601878E-14, -9.999999999999984013 ) ) ;
#3713 = DIRECTION ( 'NONE',  ( -1.000000000000000000, 5.551115123125783935E-17, -4.237045877651919561E-33 ) ) ;
#3714 = CYLINDRICAL_SURFACE ( 'NONE', #1746, 7.999999999999986677 ) ;
#3715 = CARTESIAN_POINT ( 'NONE',  ( 2.000000000000001776, -2.624548829666593232E-30, 9.999999999999998224 ) ) ;
#3716 = CARTESIAN_POINT ( 'NONE',  ( -16.49999999999996447, -102.6862915010150203, 30.68629150101515179 ) ) ;
#3717 = EDGE_LOOP ( 'NONE', ( #1681, #3261, #466, #3443 ) ) ;
#3718 = ORIENTED_EDGE ( 'NONE', *, *, #3305, .T. ) ;
#3719 = VECTOR ( 'NONE', #5301, 1000.000000000000000 ) ;
#3720 = EDGE_CURVE ( 'NONE', #6371, #3, #4726, .T. ) ;
#3721 = ADVANCED_FACE ( 'NONE', ( #65 ), #2407, .T. ) ;
#3722 = PRODUCT_DEFINITION_SHAPE ( 'NONE', 'NONE',  #1644 ) ;
#3723 = DIRECTION ( 'NONE',  ( 0.000000000000000000, 1.000000000000000000, 0.000000000000000000 ) ) ;
#3724 = CARTESIAN_POINT ( 'NONE',  ( 200.0000000000000000, 0.000000000000000000, 0.000000000000000000 ) ) ;
#3725 = FACE_OUTER_BOUND ( 'NONE', #1823, .T. ) ;
#3726 = FACE_OUTER_BOUND ( 'NONE', #5882, .T. ) ;
#3727 = CARTESIAN_POINT ( 'NONE',  ( -57.41291415210449856, -223.0630401650004728, 74.10192998188830416 ) ) ;
#3728 = DIRECTION ( 'NONE',  ( 5.605193857299270773E-45, 0.000000000000000000, 1.000000000000000000 ) ) ;
#3729 = VERTEX_POINT ( 'NONE', #2055 ) ;
#3730 = ADVANCED_FACE ( 'NONE', ( #4408 ), #217, .F. ) ;
#3731 = EDGE_CURVE ( 'NONE', #505, #4747, #6746, .T. ) ;
#3732 = ORIENTED_EDGE ( 'NONE', *, *, #5945, .T. ) ;
#3733 = DIRECTION ( 'NONE',  ( 0.000000000000000000, 0.000000000000000000, 1.000000000000000000 ) ) ;
#3734 = DIRECTION ( 'NONE',  ( 0.000000000000000000, 0.000000000000000000, 1.000000000000000000 ) ) ;
#3735 = LINE ( 'NONE', #6076, #6161 ) ;
#3736 = CARTESIAN_POINT ( 'NONE',  ( -63.29904432569978212, -218.0627255230571677, 88.88647797590476785 ) ) ;
#3737 = EDGE_LOOP ( 'NONE', ( #4821, #1293, #696, #5057 ) ) ;
#3738 = ORIENTED_EDGE ( 'NONE', *, *, #2739, .T. ) ;
#3739 =( REPRESENTATION_RELATIONSHIP ('NONE','NONE', #4862, #6475 ) REPRESENTATION_RELATIONSHIP_WITH_TRANSFORMATION ( #5205 )SHAPE_REPRESENTATION_RELATIONSHIP( ) );
#3740 = AXIS2_PLACEMENT_3D ( 'NONE', #1272, #3011, #163 ) ;
#3741 = AXIS2_PLACEMENT_3D ( 'NONE', #1757, #5845, #4775 ) ;
#3742 = CARTESIAN_POINT ( 'NONE',  ( -26.50000000000002487, -104.8363803175325444, 32.83638031753270070 ) ) ;
#3743 = CARTESIAN_POINT ( 'NONE',  ( 17.83418965632456121, -228.4878731603066910, 74.73486207509358792 ) ) ;
#3744 = VERTEX_POINT ( 'NONE', #3209 ) ;
#3745 = EDGE_CURVE ( 'NONE', #5285, #1753, #2523, .T. ) ;
#3746 = LINE ( 'NONE', #6231, #381 ) ;
#3747 = MANIFOLD_SOLID_BREP ( '<left arm>-<Fillet3>', #6265 ) ;
#3748 = CARTESIAN_POINT ( 'NONE',  ( -24.15685424949240101, 16.00000000000007105, 36.34314575050770202 ) ) ;
#3749 = TOROIDAL_SURFACE ( 'NONE', #4858, 22.00000000000000355, 3.000000000000000000 ) ;
#3750 = AXIS2_PLACEMENT_3D ( 'NONE', #6839, #1560, #6256 ) ;
#3751 = CIRCLE ( 'NONE', #1399, 6.000000000000000000 ) ;
#3752 = EDGE_LOOP ( 'NONE', ( #923, #3230 ) ) ;
#3753 = DIRECTION ( 'NONE',  ( 0.000000000000000000, -1.836970198721029934E-16, 1.000000000000000000 ) ) ;
#3754 = CIRCLE ( 'NONE', #427, 3.000000000000002665 ) ;
#3755 = FACE_OUTER_BOUND ( 'NONE', #1970, .T. ) ;
#3756 = AXIS2_PLACEMENT_3D ( 'NONE', #1364, #5527, #330 ) ;
#3757 = ORIENTED_EDGE ( 'NONE', *, *, #6132, .T. ) ;
#3758 = CYLINDRICAL_SURFACE ( 'NONE', #2243, 6.000000000000003553 ) ;
#3759 = DIRECTION ( 'NONE',  ( 0.000000000000000000, 0.000000000000000000, 1.000000000000000000 ) ) ;
#3760 = DIRECTION ( 'NONE',  ( 0.000000000000000000, 0.000000000000000000, 1.000000000000000000 ) ) ;
#3761 = AXIS2_PLACEMENT_3D ( 'NONE', #2499, #727, #1883 ) ;
#3762 = CARTESIAN_POINT ( 'NONE',  ( 2.000000000000001776, -4.040871662429601878E-14, 9.999999999999998224 ) ) ;
#3763 = DIRECTION ( 'NONE',  ( 0.000000000000000000, -1.000000000000000000, -0.000000000000000000 ) ) ;
#3764 = CARTESIAN_POINT ( 'NONE',  ( -57.47793317182449613, -223.0630299184109333, 74.12895951337506517 ) ) ;
#3765 = ORIENTED_EDGE ( 'NONE', *, *, #6176, .T. ) ;
#3766 = DIRECTION ( 'NONE',  ( -0.000000000000000000, 0.08715574274766212104, -0.9961946980917452121 ) ) ;
#3767 = EDGE_CURVE ( 'NONE', #2796, #5534, #1227, .T. ) ;
#3768 = ORIENTED_EDGE ( 'NONE', *, *, #3271, .F. ) ;
#3769 = VERTEX_POINT ( 'NONE', #1437 ) ;
#3770 = CARTESIAN_POINT ( 'NONE',  ( 1.387778780781445676E-14, 77.32233047033629703, 4.535533905932708443 ) ) ;
#3771 = CARTESIAN_POINT ( 'NONE',  ( 24.99999999999999289, 78.92893218813451028, 2.928932188134522274 ) ) ;
#3772 = CARTESIAN_POINT ( 'NONE',  ( 17.99999999999999645, 0.000000000000000000, -39.99999999999997868 ) ) ;
#3773 = AXIS2_PLACEMENT_3D ( 'NONE', #4262, #5948, #679 ) ;
#3774 = B_SPLINE_CURVE_WITH_KNOTS ( 'NONE', 3,
 ( #347, #1571, #5046, #2772 ),
 .UNSPECIFIED., .F., .F.,
 ( 4, 4 ),
 ( 3.469446951953635759E-17, 0.0007743866022177889373 ),
 .UNSPECIFIED. ) ;
#3775 = DIRECTION ( 'NONE',  ( -1.000000000000000000, 0.000000000000000000, 0.000000000000000000 ) ) ;
#3776 = EDGE_CURVE ( 'NONE', #4453, #3147, #175, .T. ) ;
#3777 = ORIENTED_EDGE ( 'NONE', *, *, #1072, .F. ) ;
#3778 = EDGE_LOOP ( 'NONE', ( #758, #1319, #4719, #5507 ) ) ;
#3779 =( BOUNDED_CURVE ( )  B_SPLINE_CURVE ( 3, ( #6549, #4276, #5926, #7040 ),
 .UNSPECIFIED., .F., .T. ) 
 B_SPLINE_CURVE_WITH_KNOTS ( ( 4, 4 ),
 ( 3.926990816987244060, 4.712388980384692339 ),
 .UNSPECIFIED. ) 
 CURVE ( )  GEOMETRIC_REPRESENTATION_ITEM ( )  RATIONAL_B_SPLINE_CURVE ( ( 1.000000000000000000, 0.9492530216741911220, 0.9492530216741911220, 1.000000000000000000 ) ) 
 REPRESENTATION_ITEM ( '' )  );
#3780 = CIRCLE ( 'NONE', #6716, 3.000000000000002665 ) ;
#3781 = CARTESIAN_POINT ( 'NONE',  ( 27.21559789597881007, -217.6453243769068706, 77.74120035865662715 ) ) ;
#3782 = ORIENTED_EDGE ( 'NONE', *, *, #2898, .T. ) ;
#3783 = DIRECTION ( 'NONE',  ( 0.7660444431189621373, 1.387778780781445676E-17, 0.6427876096865583477 ) ) ;
#3784 = CARTESIAN_POINT ( 'NONE',  ( -29.64230087749237086, -110.3978942797115650, 38.39789427971174263 ) ) ;
#3785 = CIRCLE ( 'NONE', #2915, 2.999999999999999112 ) ;
#3786 = ORIENTED_EDGE ( 'NONE', *, *, #6522, .F. ) ;
#3787 = EDGE_CURVE ( 'NONE', #245, #3851, #855, .T. ) ;
#3788 = CARTESIAN_POINT ( 'NONE',  ( 21.50000000000000000, -104.1739323729103432, 75.12787131935894536 ) ) ;
#3789 = CARTESIAN_POINT ( 'NONE',  ( 3.000000000000002665, -60.00000000000000000, 3.000000000000000000 ) ) ;
#3790 = DIRECTION ( 'NONE',  ( -1.000000000000000000, 0.000000000000000000, 0.000000000000000000 ) ) ;
#3791 = VERTEX_POINT ( 'NONE', #3716 ) ;
#3792 = LINE ( 'NONE', #4328, #5434 ) ;
#3793 = CARTESIAN_POINT ( 'NONE',  ( 53.00000000000000711, 4.543323389463065786E-15, 13.00000000000001066 ) ) ;
#3794 = DIRECTION ( 'NONE',  ( 0.000000000000000000, 0.000000000000000000, 1.000000000000000000 ) ) ;
#3795 = ORIENTED_EDGE ( 'NONE', *, *, #1198, .T. ) ;
#3796 = EDGE_LOOP ( 'NONE', ( #4405, #1280, #5296, #7405 ) ) ;
#3797 = EDGE_CURVE ( 'NONE', #1310, #2601, #976, .T. ) ;
#3798 = CARTESIAN_POINT ( 'NONE',  ( 21.50000000000000000, 0.000000000000000000, 5.999999999999999112 ) ) ;
#3799 =( LENGTH_UNIT ( ) NAMED_UNIT ( * ) SI_UNIT ( .MILLI., .METRE. ) );
#3800 = LINE ( 'NONE', #2561, #7553 ) ;
#3801 = CARTESIAN_POINT ( 'NONE',  ( -57.12880255235567972, -223.0631510105118309, 73.98989896671450595 ) ) ;
#3802 = CARTESIAN_POINT ( 'NONE',  ( 187.5208673656504175, -7.524439173533908232, 15.00000000000001066 ) ) ;
#3803 = CARTESIAN_POINT ( 'NONE',  ( -64.50000000000000000, -7.347880794884119736E-16, -6.000000000000000000 ) ) ;
#3804 = EDGE_LOOP ( 'NONE', ( #6837, #5275, #7234, #3519 ) ) ;
#3805 = ORIENTED_EDGE ( 'NONE', *, *, #4421, .F. ) ;
#3806 = ADVANCED_FACE ( 'NONE', ( #4330 ), #5488, .F. ) ;
#3807 = CARTESIAN_POINT ( 'NONE',  ( 50.00000000000000000, 15.08392021690038121, 15.00000000000000888 ) ) ;
#3808 = DIRECTION ( 'NONE',  ( 0.000000000000000000, -0.08715574274766212104, 0.9961946980917452121 ) ) ;
#3809 = LINE ( 'NONE', #6178, #512 ) ;
#3810 = ORIENTED_EDGE ( 'NONE', *, *, #6700, .F. ) ;
#3811 = VERTEX_POINT ( 'NONE', #1978 ) ;
#3812 = CLOSED_SHELL ( 'NONE', ( #7317, #6887, #2545, #345, #2020, #6609, #5031, #3721, #4981, #1763, #5581, #1271, #815, #6545 ) ) ;
#3813 = ADVANCED_FACE ( 'NONE', ( #6671 ), #1394, .F. ) ;
#3814 = EDGE_CURVE ( 'NONE', #5579, #3936, #4952, .T. ) ;
#3815 = DIRECTION ( 'NONE',  ( -1.000000000000000000, -0.000000000000000000, -0.000000000000000000 ) ) ;
#3816 = EDGE_LOOP ( 'NONE', ( #2050, #6079, #1038, #5282 ) ) ;
#3817 = DIRECTION ( 'NONE',  ( 5.551115123125783935E-17, -0.7071067811865469066, -0.7071067811865481278 ) ) ;
#3818 = DIRECTION ( 'NONE',  ( 1.000000000000000000, 0.000000000000000000, 0.000000000000000000 ) ) ;
#3819 = AXIS2_PLACEMENT_3D ( 'NONE', #5668, #2666, #2701 ) ;
#3820 =( BOUNDED_CURVE ( )  B_SPLINE_CURVE ( 3, ( #2799, #4501, #4657, #3998 ),
 .UNSPECIFIED., .F., .T. ) 
 B_SPLINE_CURVE_WITH_KNOTS ( ( 4, 4 ),
 ( 1.570796326794896558, 3.141592653589793116 ),
 .UNSPECIFIED. ) 
 CURVE ( )  GEOMETRIC_REPRESENTATION_ITEM ( )  RATIONAL_B_SPLINE_CURVE ( ( 1.000000000000000000, 0.8047378541243649375, 0.8047378541243649375, 1.000000000000000000 ) ) 
 REPRESENTATION_ITEM ( '' )  );
#3821 = ORIENTED_EDGE ( 'NONE', *, *, #5058, .T. ) ;
#3822 = EDGE_CURVE ( 'NONE', #7561, #2908, #2074, .T. ) ;
#3823 = CARTESIAN_POINT ( 'NONE',  ( 0.000000000000000000, 0.000000000000000000, -9.999999999999994671 ) ) ;
#3824 = AXIS2_PLACEMENT_3D ( 'NONE', #2386, #4749, #6041 ) ;
#3825 = DIRECTION ( 'NONE',  ( 1.000000000000000000, 2.465190328815661892E-32, -9.244463733058732095E-33 ) ) ;
#3826 = CARTESIAN_POINT ( 'NONE',  ( 185.0000000000000000, 39.99999999999999289, 10.00000000000000355 ) ) ;
#3827 = ORIENTED_EDGE ( 'NONE', *, *, #1839, .T. ) ;
#3828 =( NAMED_UNIT ( * ) PLANE_ANGLE_UNIT ( ) SI_UNIT ( $, .RADIAN. ) );
#3829 = DIRECTION ( 'NONE',  ( -0.000000000000000000, 1.000000000000000000, 3.304235192336776498E-16 ) ) ;
#3830 = FACE_OUTER_BOUND ( 'NONE', #4339, .T. ) ;
#3831 = DIRECTION ( 'NONE',  ( 1.000000000000000000, 0.000000000000000000, 0.000000000000000000 ) ) ;
#3832 = PRESENTATION_LAYER_ASSIGNMENT (  '', '', ( #7145 ) ) ;
#3833 = VERTEX_POINT ( 'NONE', #5023 ) ;
#3834 = CYLINDRICAL_SURFACE ( 'NONE', #573, 10.00000000000000355 ) ;
#3835 = AXIS2_PLACEMENT_3D ( 'NONE', #2053, #5486, #2588 ) ;
#3836 = CARTESIAN_POINT ( 'NONE',  ( 0.000000000000000000, 0.000000000000000000, 0.000000000000000000 ) ) ;
#3837 = CARTESIAN_POINT ( 'NONE',  ( 26.00000000000000000, -2.887003712633254693E-29, 6.000000000000000888 ) ) ;
#3838 = DIRECTION ( 'NONE',  ( -1.000000000000000000, 0.000000000000000000, -7.663350976776343357E-46 ) ) ;
#3839 = CARTESIAN_POINT ( 'NONE',  ( -58.82507573250082089, -223.0635350528836511, 74.77305146519802292 ) ) ;
#3840 = DIRECTION ( 'NONE',  ( 0.000000000000000000, 1.000000000000000000, 0.000000000000000000 ) ) ;
#3841 = CARTESIAN_POINT ( 'NONE',  ( 170.0000000000000000, 11.00000000000000711, 8.660254037844383745 ) ) ;
#3842 = EDGE_CURVE ( 'NONE', #5048, #917, #970, .T. ) ;
#3843 = VECTOR ( 'NONE', #5806, 1000.000000000000000 ) ;
#3844 = ORIENTED_EDGE ( 'NONE', *, *, #5539, .F. ) ;
#3845 = ORIENTED_EDGE ( 'NONE', *, *, #327, .T. ) ;
#3846 = FACE_OUTER_BOUND ( 'NONE', #4357, .T. ) ;
#3847 = DIRECTION ( 'NONE',  ( 5.605193857299270773E-45, 0.000000000000000000, 1.000000000000000000 ) ) ;
#3848 = CARTESIAN_POINT ( 'NONE',  ( -26.50000000000000711, -117.9145199278634806, 44.76505905230362714 ) ) ;
#3849 = EDGE_CURVE ( 'NONE', #7257, #1936, #5039, .T. ) ;
#3850 = VERTEX_POINT ( 'NONE', #7394 ) ;
#3851 = VERTEX_POINT ( 'NONE', #4023 ) ;
#3852 = CIRCLE ( 'NONE', #4720, 10.00000000000000711 ) ;
#3853 = CARTESIAN_POINT ( 'NONE',  ( -22.93100982128538234, -73.43085575620197858, 46.43085575620212069 ) ) ;
#3854 = VERTEX_POINT ( 'NONE', #4442 ) ;
#3855 = LINE ( 'NONE', #5080, #1731 ) ;
#3856 = CARTESIAN_POINT ( 'NONE',  ( 220.0000000000000000, 56.99999999999999289, 10.00000000000002132 ) ) ;
#3857 = EDGE_CURVE ( 'NONE', #4957, #7205, #6019, .T. ) ;
#3858 = EDGE_LOOP ( 'NONE', ( #2127, #6912 ) ) ;
#3859 = CIRCLE ( 'NONE', #533, 3.000000000000000000 ) ;
#3860 = LINE ( 'NONE', #3788, #4027 ) ;
#3861 = CARTESIAN_POINT ( 'NONE',  ( 48.51085693943250021, 26.66014758463033729, 12.77153349490077794 ) ) ;
#3862 = VERTEX_POINT ( 'NONE', #1050 ) ;
#3863 = CARTESIAN_POINT ( 'NONE',  ( 0.000000000000000000, 0.000000000000000000, 0.000000000000000000 ) ) ;
#3864 = LINE ( 'NONE', #4555, #5066 ) ;
#3865 =( GEOMETRIC_REPRESENTATION_CONTEXT ( 3 ) GLOBAL_UNCERTAINTY_ASSIGNED_CONTEXT ( ( #5185 ) ) GLOBAL_UNIT_ASSIGNED_CONTEXT ( ( #4108, #2948, #4412 ) ) REPRESENTATION_CONTEXT ( 'NONE', 'WORKASPACE' ) );
#3866 = LINE ( 'NONE', #891, #493 ) ;
#3867 = DIRECTION ( 'NONE',  ( 0.5773502691896309491, -0.5773502691896224004, 0.5773502691896238437 ) ) ;
#3868 = EDGE_CURVE ( 'NONE', #5394, #2971, #3410, .T. ) ;
#3869 = ORIENTED_EDGE ( 'NONE', *, *, #1836, .F. ) ;
#3870 = AXIS2_PLACEMENT_3D ( 'NONE', #120, #2382, #4850 ) ;
#3871 = CIRCLE ( 'NONE', #1780, 2.999999999999999112 ) ;
#3872 = AXIS2_PLACEMENT_3D ( 'NONE', #2202, #350, #6196 ) ;
#3873 = FACE_BOUND ( 'NONE', #5971, .T. ) ;
#3874 = CARTESIAN_POINT ( 'NONE',  ( 217.0000000000000000, -3.000000000000000000, 35.00000000000000000 ) ) ;
#3875 = CARTESIAN_POINT ( 'NONE',  ( 189.0640241484130968, 7.505526787993156645, 15.36891305950205577 ) ) ;
#3876 = CARTESIAN_POINT ( 'NONE',  ( -60.25732134435390464, -223.0624617060423986, 93.74339436655736790 ) ) ;
#3877 = CARTESIAN_POINT ( 'NONE',  ( -14.84314575050763096, -218.0630240738404666, 95.20959099461347819 ) ) ;
#3878 = CYLINDRICAL_SURFACE ( 'NONE', #2695, 3.000000000000007994 ) ;
#3879 = VECTOR ( 'NONE', #2617, 1000.000000000000000 ) ;
#3881 = CARTESIAN_POINT ( 'NONE',  ( -61.77318701999629980, -218.0630240738405234, 91.25301986902242390 ) ) ;
#3880 = CIRCLE ( 'NONE', #2761, 3.000000000000000888 ) ;
#3882 = ORIENTED_EDGE ( 'NONE', *, *, #219, .F. ) ;
#3883 = ORIENTED_EDGE ( 'NONE', *, *, #7005, .T. ) ;
#3884 = EDGE_CURVE ( 'NONE', #5471, #312, #7496, .T. ) ;
#3885 = DIRECTION ( 'NONE',  ( 0.000000000000000000, 0.000000000000000000, 1.000000000000000000 ) ) ;
#3886 = CARTESIAN_POINT ( 'NONE',  ( -53.21539232130207608, -222.1285142276788065, 73.03087698472252498 ) ) ;
#3887 = ADVANCED_FACE ( 'NONE', ( #1545 ), #5134, .T. ) ;
#3888 = DIRECTION ( 'NONE',  ( 0.000000000000000000, -0.9961946980917452121, -0.08715574274766212104 ) ) ;
#3889 = CARTESIAN_POINT ( 'NONE',  ( -64.50000000000000000, -6.938893903907228378E-15, -15.99999999999998579 ) ) ;
#3890 = APPLICATION_CONTEXT ( 'automotive_design' ) ;
#3891 = ORIENTED_EDGE ( 'NONE', *, *, #1836, .T. ) ;
#3892 = VERTEX_POINT ( 'NONE', #6282 ) ;
#3893 = EDGE_CURVE ( 'NONE', #1572, #245, #4481, .T. ) ;
#3894 = PLANE ( 'NONE',  #5334 ) ;
#3895 = ORIENTED_EDGE ( 'NONE', *, *, #2533, .T. ) ;
#3896 = PLANE ( 'NONE',  #7501 ) ;
#3897 = CARTESIAN_POINT ( 'NONE',  ( -18.49999999999999289, 16.00000000000007105, 30.68629150101529035 ) ) ;
#3898 = ORIENTED_EDGE ( 'NONE', *, *, #4810, .T. ) ;
#3899 = EDGE_CURVE ( 'NONE', #3492, #1345, #3240, .T. ) ;
#3900 = ADVANCED_FACE ( 'NONE', ( #1010 ), #5171, .F. ) ;
#3901 = CARTESIAN_POINT ( 'NONE',  ( 51.79800105182918912, 27.71015215774388096, 10.00000000000000888 ) ) ;
#3902 = FACE_OUTER_BOUND ( 'NONE', #3796, .T. ) ;
#3903 = EDGE_LOOP ( 'NONE', ( #6108, #6109 ) ) ;
#3904 = AXIS2_PLACEMENT_3D ( 'NONE', #2740, #3561, #5869 ) ;
#3905 = DIRECTION ( 'NONE',  ( 4.063105514724585671E-29, 1.000000000000000000, -1.196959198424002812E-16 ) ) ;
#3906 = CARTESIAN_POINT ( 'NONE',  ( -60.66745985056437007, -212.4343899438517269, 94.21711093295449757 ) ) ;
#3907 = CARTESIAN_POINT ( 'NONE',  ( 209.9999999999999716, 6.000000000000000000, 41.00000000000002132 ) ) ;
#3908 = CARTESIAN_POINT ( 'NONE',  ( -21.49999999999999289, 16.00000000000004263, 42.31370849898488729 ) ) ;
#3909 = ORIENTED_EDGE ( 'NONE', *, *, #2430, .F. ) ;
#3910 = ORIENTED_EDGE ( 'NONE', *, *, #6768, .F. ) ;
#3911 = DIRECTION ( 'NONE',  ( -1.007940753403772230E-16, 0.08715574274766275942, -0.9961946980917452121 ) ) ;
#3912 = EDGE_CURVE ( 'NONE', #131, #4590, #7510, .T. ) ;
#3913 = DIRECTION ( 'NONE',  ( 4.036065081973857683E-17, 0.03489949670250346025, 0.9993908270190956511 ) ) ;
#3914 = FACE_OUTER_BOUND ( 'NONE', #2934, .T. ) ;
#3915 = CARTESIAN_POINT ( 'NONE',  ( -14.00000000000000000, 1.714505518806294046E-15, -9.999999999999994671 ) ) ;
#3916 = DIRECTION ( 'NONE',  ( 1.000000000000000000, 0.000000000000000000, 0.000000000000000000 ) ) ;
#3917 = CARTESIAN_POINT ( 'NONE',  ( 30.00000000000000000, -2.624548829666611800E-30, 8.000000000000000000 ) ) ;
#3918 = ORIENTED_EDGE ( 'NONE', *, *, #4663, .F. ) ;
#3919 = EDGE_LOOP ( 'NONE', ( #5432, #3932, #5147, #2965 ) ) ;
#3920 = DIRECTION ( 'NONE',  ( 0.000000000000000000, 0.000000000000000000, -1.000000000000000000 ) ) ;
#3921 = FACE_OUTER_BOUND ( 'NONE', #3919, .T. ) ;
#3922 = CARTESIAN_POINT ( 'NONE',  ( 0.000000000000000000, 0.000000000000000000, 0.000000000000000000 ) ) ;
#3923 = DIRECTION ( 'NONE',  ( 0.000000000000000000, 1.000000000000000000, 0.000000000000000000 ) ) ;
#3924 = CARTESIAN_POINT ( 'NONE',  ( -16.49999999999998224, -69.36092951174981636, 42.36092951174991583 ) ) ;
#3925 = ORIENTED_EDGE ( 'NONE', *, *, #4586, .T. ) ;
#3926 = ORIENTED_EDGE ( 'NONE', *, *, #1430, .F. ) ;
#3927 = CARTESIAN_POINT ( 'NONE',  ( 2.775557561562891351E-14, 40.21320343559642652, 10.99999999999999467 ) ) ;
#3928 = ORIENTED_EDGE ( 'NONE', *, *, #928, .T. ) ;
#3929 = DIRECTION ( 'NONE',  ( 0.000000000000000000, 0.000000000000000000, 1.000000000000000000 ) ) ;
#3930 = DIRECTION ( 'NONE',  ( -1.000000000000000000, 0.000000000000000000, 0.000000000000000000 ) ) ;
#3931 = EDGE_CURVE ( 'NONE', #4614, #7465, #6941, .T. ) ;
#3932 = ORIENTED_EDGE ( 'NONE', *, *, #6758, .F. ) ;
#3933 = AXIS2_PLACEMENT_3D ( 'NONE', #2867, #6251, #7559 ) ;
#3934 = CARTESIAN_POINT ( 'NONE',  ( 53.00000000000002132, -18.00000000000000000, 10.00000000000000888 ) ) ;
#3935 = LINE ( 'NONE', #3285, #7304 ) ;
#3936 = VERTEX_POINT ( 'NONE', #5631 ) ;
#3937 = CARTESIAN_POINT ( 'NONE',  ( 203.9378221735088630, -6.000000000000000000, 38.50000000000000000 ) ) ;
#3938 = TOROIDAL_SURFACE ( 'NONE', #2212, 6.000000000000000000, 3.000000000000000000 ) ;
#3939 = DIRECTION ( 'NONE',  ( 0.000000000000000000, 0.000000000000000000, 1.000000000000000000 ) ) ;
#3940 = AXIS2_PLACEMENT_3D ( 'NONE', #6722, #2600, #2564 ) ;
#3941 = CARTESIAN_POINT ( 'NONE',  ( -64.50000000000000000, -6.938893903907228378E-15, -15.99999999999998579 ) ) ;
#3942 = EDGE_CURVE ( 'NONE', #529, #2192, #1632, .T. ) ;
#3943 = ORIENTED_EDGE ( 'NONE', *, *, #5243, .T. ) ;
#3944 = VERTEX_POINT ( 'NONE', #6823 ) ;
#3945 = TOROIDAL_SURFACE ( 'NONE', #4433, 22.00000000000000355, 3.000000000000000000 ) ;
#3946 = CARTESIAN_POINT ( 'NONE',  ( 25.00000000000002842, 33.14213562373094391, 8.071067811865434649 ) ) ;
#3947 =( NAMED_UNIT ( * ) PLANE_ANGLE_UNIT ( ) SI_UNIT ( $, .RADIAN. ) );
#3948 = LINE ( 'NONE', #362, #5230 ) ;
#3949 = DIRECTION ( 'NONE',  ( 4.622231866529368100E-33, -2.600005424922769496E-32, 1.000000000000000000 ) ) ;
#3950 = ORIENTED_EDGE ( 'NONE', *, *, #1521, .T. ) ;
#3951 = DIRECTION ( 'NONE',  ( 1.000000000000000000, 2.465190328815661892E-32, -9.244463733058732095E-33 ) ) ;
#3952 = VECTOR ( 'NONE', #2117, 999.9999999999998863 ) ;
#3953 = CARTESIAN_POINT ( 'NONE',  ( -60.56776133228527925, -218.0630240738405234, 74.80990615958565115 ) ) ;
#3954 = EDGE_CURVE ( 'NONE', #3477, #228, #2170, .T. ) ;
#3955 = ORIENTED_EDGE ( 'NONE', *, *, #1542, .F. ) ;
#3956 = EDGE_LOOP ( 'NONE', ( #766, #3254, #2209, #3183 ) ) ;
#3957 = CARTESIAN_POINT ( 'NONE',  ( 14.52070450238005606, -218.0630240738404666, 72.88438438556153187 ) ) ;
#3958 = CARTESIAN_POINT ( 'NONE',  ( -29.35769912250765046, 16.00000000000004263, 38.63670350735201708 ) ) ;
#3959 = CARTESIAN_POINT ( 'NONE',  ( 185.0000000000000000, 39.99999999999999289, 0.000000000000000000 ) ) ;
#3960 = DIRECTION ( 'NONE',  ( 4.622231866529368100E-33, -2.600005424922769496E-32, 1.000000000000000000 ) ) ;
#3961 = FACE_OUTER_BOUND ( 'NONE', #4627, .T. ) ;
#3962 = AXIS2_PLACEMENT_3D ( 'NONE', #4003, #1105, #2720 ) ;
#3963 = EDGE_CURVE ( 'NONE', #6542, #4415, #5940, .T. ) ;
#3964 = ORIENTED_EDGE ( 'NONE', *, *, #4949, .T. ) ;
#3965 = ORIENTED_EDGE ( 'NONE', *, *, #2870, .T. ) ;
#3966 = LINE ( 'NONE', #4083, #2275 ) ;
#3967 = ORIENTED_EDGE ( 'NONE', *, *, #2621, .F. ) ;
#3968 = DIRECTION ( 'NONE',  ( 0.000000000000000000, -0.08715574274766212104, 0.9961946980917452121 ) ) ;
#3969 = CARTESIAN_POINT ( 'NONE',  ( 50.00000000000000000, -22.89008536370704050, 9.895301509892497904 ) ) ;
#3970 = ORIENTED_EDGE ( 'NONE', *, *, #6522, .T. ) ;
#3971 = VECTOR ( 'NONE', #4177, 1000.000000000000000 ) ;
#3972 = EDGE_CURVE ( 'NONE', #7420, #5285, #6923, .T. ) ;
#3973 = DIRECTION ( 'NONE',  ( -7.663350976776344912E-46, 0.000000000000000000, -1.000000000000000000 ) ) ;
#3974 = FACE_OUTER_BOUND ( 'NONE', #4886, .T. ) ;
#3975 = ORIENTED_EDGE ( 'NONE', *, *, #3711, .T. ) ;
#3976 = DIRECTION ( 'NONE',  ( -0.9850390035862324201, -1.421202942680585964E-17, -0.1723315450341066923 ) ) ;
#3977 = CARTESIAN_POINT ( 'NONE',  ( -60.73846410710429211, -217.2436419687046509, 95.06511182196476284 ) ) ;
#3978 = DIRECTION ( 'NONE',  ( -0.000000000000000000, 1.000000000000000000, 3.304235192336776498E-16 ) ) ;
#3979 = CARTESIAN_POINT ( 'NONE',  ( -26.50000000000000711, -117.9145199278634806, 44.76505905230362714 ) ) ;
#3980 = VECTOR ( 'NONE', #5710, 1000.000000000000000 ) ;
#3981 = ORIENTED_EDGE ( 'NONE', *, *, #5594, .F. ) ;
#3982 = ORIENTED_EDGE ( 'NONE', *, *, #4586, .F. ) ;
#3983 = CARTESIAN_POINT ( 'NONE',  ( 0.000000000000000000, 56.99999999999999289, 7.000000000000022204 ) ) ;
#3984 = AXIS2_PLACEMENT_3D ( 'NONE', #767, #1887, #2969 ) ;
#3985 = PRESENTATION_LAYER_ASSIGNMENT (  '', '', ( #786 ) ) ;
#3986 = DIRECTION ( 'NONE',  ( 1.000000000000000000, 2.624548829666596736E-30, -9.231085635203017994E-31 ) ) ;
#3987 = CARTESIAN_POINT ( 'NONE',  ( 186.4659479370544375, 6.011053575986605502, 14.23782611900703010 ) ) ;
#3988 = CARTESIAN_POINT ( 'NONE',  ( -53.47314606205194565, -223.0630240738404950, 96.09122589815579829 ) ) ;
#3989 = CARTESIAN_POINT ( 'NONE',  ( 20.03634105971836377, -223.0630240738403813, 78.93565216506947024 ) ) ;
#3990 = DIRECTION ( 'NONE',  ( -0.8660254037844404840, 0.000000000000000000, 0.4999999999999968359 ) ) ;
#3991 = CARTESIAN_POINT ( 'NONE',  ( -63.63476818105571908, -218.0630489433316370, 79.22587972011848478 ) ) ;
#3992 = CIRCLE ( 'NONE', #1285, 3.000000000000002665 ) ;
#3993 = VERTEX_POINT ( 'NONE', #5096 ) ;
#3994 = VERTEX_POINT ( 'NONE', #7587 ) ;
#3995 = CARTESIAN_POINT ( 'NONE',  ( 209.9999999999999716, 6.000000000000000000, 35.00000000000000000 ) ) ;
#3996 = DIRECTION ( 'NONE',  ( 0.000000000000000000, 2.065146995210484941E-16, -1.000000000000000000 ) ) ;
#3997 = AXIS2_PLACEMENT_3D ( 'NONE', #991, #5152, #7490 ) ;
#3998 = CARTESIAN_POINT ( 'NONE',  ( -13.49999999999999822, -223.0630240738404666, 96.09122589815579829 ) ) ;
#3999 = DIRECTION ( 'NONE',  ( -1.000000000000000000, 0.000000000000000000, 0.000000000000000000 ) ) ;
#4000 = VECTOR ( 'NONE', #5016, 1000.000000000000114 ) ;
#4001 = EDGE_CURVE ( 'NONE', #570, #6714, #6404, .T. ) ;
#4002 = CIRCLE ( 'NONE', #4486, 2.999999999999999112 ) ;
#4003 = CARTESIAN_POINT ( 'NONE',  ( -16.49999999999996447, -49.37258300203045280, -2.775557561562891351E-14 ) ) ;
#4004 = EDGE_LOOP ( 'NONE', ( #3196, #35, #2544, #1031 ) ) ;
#4005 = EDGE_CURVE ( 'NONE', #4710, #3162, #556, .T. ) ;
#4006 = ORIENTED_EDGE ( 'NONE', *, *, #6203, .T. ) ;
#4007 = DIRECTION ( 'NONE',  ( 0.000000000000000000, 0.000000000000000000, -1.000000000000000000 ) ) ;
#4008 = LINE ( 'NONE', #3310, #6574 ) ;
#4009 = ADVANCED_FACE ( 'NONE', ( #1822 ), #2611, .T. ) ;
#4010 = EDGE_LOOP ( 'NONE', ( #2003, #6511, #6350, #6238 ) ) ;
#4011 = CARTESIAN_POINT ( 'NONE',  ( 188.6380400399839061, -7.242640687119284770, 15.00000000000001066 ) ) ;
#4012 = EDGE_LOOP ( 'NONE', ( #1988, #6911, #5474, #7522 ) ) ;
#4013 = DIRECTION ( 'NONE',  ( 5.605193857299270773E-45, 0.000000000000000000, 1.000000000000000000 ) ) ;
#4014 = EDGE_CURVE ( 'NONE', #5692, #3401, #2437, .T. ) ;
#4015 = ORIENTED_EDGE ( 'NONE', *, *, #6333, .F. ) ;
#4016 = ORIENTED_EDGE ( 'NONE', *, *, #3349, .T. ) ;
#4017 = VECTOR ( 'NONE', #2568, 1000.000000000000000 ) ;
#4018 = DIRECTION ( 'NONE',  ( -2.465190328815661892E-32, -1.000000000000000000, -1.193489751472043281E-15 ) ) ;
#4019 = FACE_OUTER_BOUND ( 'NONE', #2434, .T. ) ;
#4020 = ORIENTED_EDGE ( 'NONE', *, *, #6492, .F. ) ;
#4021 = CARTESIAN_POINT ( 'NONE',  ( 201.4915464889351426, -19.99999999999930012, 83.63391996479855095 ) ) ;
#4022 = CARTESIAN_POINT ( 'NONE',  ( 170.0000000000000000, -10.56957438397690474, -9.180637088000993984 ) ) ;
#4023 = CARTESIAN_POINT ( 'NONE',  ( 2.000000000000001776, 1.224646799147350101E-15, -9.999999999999998224 ) ) ;
#4024 = AXIS2_PLACEMENT_3D ( 'NONE', #3103, #2707, #328 ) ;
#4025 = ORIENTED_EDGE ( 'NONE', *, *, #4094, .F. ) ;
#4026 = ORIENTED_EDGE ( 'NONE', *, *, #3483, .F. ) ;
#4027 = VECTOR ( 'NONE', #5553, 1000.000000000000000 ) ;
#4028 = CARTESIAN_POINT ( 'NONE',  ( 21.50000000000000000, -120.9522879036832848, 45.92078884797942351 ) ) ;
#4029 = CARTESIAN_POINT ( 'NONE',  ( 176.5000000000000000, -39.99999999999999289, 10.00000000000000355 ) ) ;
#4030 = DIRECTION ( 'NONE',  ( -1.000000000000000000, 0.000000000000000000, 0.000000000000000000 ) ) ;
#4031 = CARTESIAN_POINT ( 'NONE',  ( -61.43119716943146358, -223.0630215652982713, 92.62836485985936008 ) ) ;
#4032 = CARTESIAN_POINT ( 'NONE',  ( 18.63431107999237923, -223.0630240738404666, 92.40830921507968299 ) ) ;
#4033 = CARTESIAN_POINT ( 'NONE',  ( -16.49999999999998934, -71.76505905230354188, 44.76505905230365556 ) ) ;
#4034 = CARTESIAN_POINT ( 'NONE',  ( -62.03747301282925974, -218.0635026243406287, 76.42168781368546604 ) ) ;
#4035 = EDGE_CURVE ( 'NONE', #2698, #5113, #5936, .T. ) ;
#4036 = APPLICATION_CONTEXT ( 'automotive_design' ) ;
#4037 = VERTEX_POINT ( 'NONE', #5897 ) ;
#4038 = DIRECTION ( 'NONE',  ( 1.000000000000000000, 0.000000000000000000, 0.000000000000000000 ) ) ;
#4039 = CARTESIAN_POINT ( 'NONE',  ( 217.0000000000000000, -5.510910596163110263E-16, 3.000000000000011102 ) ) ;
#4040 = CARTESIAN_POINT ( 'NONE',  ( 4.000000000000003553, 0.000000000000000000, 1.387778780781445676E-14 ) ) ;
#4041 = FACE_OUTER_BOUND ( 'NONE', #3533, .T. ) ;
#4042 = LINE ( 'NONE', #2762, #4451 ) ;
#4043 = EDGE_CURVE ( 'NONE', #6224, #3543, #3114, .T. ) ;
#4044 = ORIENTED_EDGE ( 'NONE', *, *, #7295, .T. ) ;
#4045 = ORIENTED_EDGE ( 'NONE', *, *, #6213, .T. ) ;
#4046 = DIRECTION ( 'NONE',  ( 0.000000000000000000, 0.000000000000000000, 1.000000000000000000 ) ) ;
#4047 = ORIENTED_EDGE ( 'NONE', *, *, #1878, .F. ) ;
#4048 = CARTESIAN_POINT ( 'NONE',  ( -26.50000000000000711, -71.76505905230354188, 44.76505905230365556 ) ) ;
#4049 = DIRECTION ( 'NONE',  ( 0.000000000000000000, 0.000000000000000000, -1.000000000000000000 ) ) ;
#4050 = ORIENTED_EDGE ( 'NONE', *, *, #909, .T. ) ;
#4051 = EDGE_CURVE ( 'NONE', #7274, #3854, #6061, .T. ) ;
#4052 = EDGE_CURVE ( 'NONE', #5611, #7449, #3852, .T. ) ;
#4053 = ORIENTED_EDGE ( 'NONE', *, *, #7431, .T. ) ;
#4054 = DIRECTION ( 'NONE',  ( -0.000000000000000000, -1.000000000000000000, -2.065146995210484941E-16 ) ) ;
#4055 = DIRECTION ( 'NONE',  ( 0.000000000000000000, 0.000000000000000000, -1.000000000000000000 ) ) ;
#4056 = ORIENTED_EDGE ( 'NONE', *, *, #2917, .F. ) ;
#4057 = DIRECTION ( 'NONE',  ( 1.000000000000000000, 0.000000000000000000, 0.000000000000000000 ) ) ;
#4058 = DIRECTION ( 'NONE',  ( -9.860761315262649757E-32, 1.000000000000000000, 0.000000000000000000 ) ) ;
#4059 = AXIS2_PLACEMENT_3D ( 'NONE', #1828, #3606, #4186 ) ;
#4060 = ORIENTED_EDGE ( 'NONE', *, *, #4917, .F. ) ;
#4061 = ADVANCED_FACE ( 'NONE', ( #3018 ), #4717, .F. ) ;
#4062 = DIRECTION ( 'NONE',  ( -0.5773502691896310601, -0.5773502691896222894, 0.5773502691896238437 ) ) ;
#4063 = CIRCLE ( 'NONE', #2340, 2.999999999999999112 ) ;
#4064 = CARTESIAN_POINT ( 'NONE',  ( 217.0000000000000000, -3.000000000000000888, 18.00000000000001066 ) ) ;
#4065 = VECTOR ( 'NONE', #3221, 1000.000000000000000 ) ;
#4066 = CARTESIAN_POINT ( 'NONE',  ( 16.72842210847736766, -218.0630240738404950, 74.10707748653940996 ) ) ;
#4067 = DIRECTION ( 'NONE',  ( 0.000000000000000000, 0.000000000000000000, -1.000000000000000000 ) ) ;
#4068 = CARTESIAN_POINT ( 'NONE',  ( -64.50000000000000000, -45.34314575050760254, 18.34314575050763452 ) ) ;
#4069 = AXIS2_PLACEMENT_3D ( 'NONE', #934, #1543, #1501 ) ;
#4070 = ORIENTED_EDGE ( 'NONE', *, *, #4334, .F. ) ;
#4071 = ORIENTED_EDGE ( 'NONE', *, *, #5323, .F. ) ;
#4072 = FILL_AREA_STYLE ('',( #6533 ) ) ;
#4073 = CYLINDRICAL_SURFACE ( 'NONE', #3402, 6.000000000000001776 ) ;
#4074 = LINE ( 'NONE', #6571, #2282 ) ;
#4075 = EDGE_CURVE ( 'NONE', #7239, #7538, #528, .T. ) ;
#4076 = CARTESIAN_POINT ( 'NONE',  ( 187.1032342689625523, 6.494950219283388115, 15.00000000000001066 ) ) ;
#4077 = AXIS2_PLACEMENT_3D ( 'NONE', #6772, #3197, #881 ) ;
#4078 = ADVANCED_FACE ( 'NONE', ( #1277 ), #2292, .T. ) ;
#4079 = CARTESIAN_POINT ( 'NONE',  ( 220.0000000000000000, -60.00000000000000000, 7.000000000000000000 ) ) ;
#4080 = VERTEX_POINT ( 'NONE', #627 ) ;
#4081 = ORIENTED_EDGE ( 'NONE', *, *, #941, .T. ) ;
#4082 = EDGE_CURVE ( 'NONE', #4118, #1397, #4641, .T. ) ;
#4083 = CARTESIAN_POINT ( 'NONE',  ( 193.5000000000000000, 39.99999999999999289, 0.000000000000000000 ) ) ;
#4084 = ORIENTED_EDGE ( 'NONE', *, *, #3849, .F. ) ;
#4085 = DIRECTION ( 'NONE',  ( 0.000000000000000000, 0.000000000000000000, -1.000000000000000000 ) ) ;
#4086 = LINE ( 'NONE', #4785, #192 ) ;
#4087 = ORIENTED_EDGE ( 'NONE', *, *, #4117, .F. ) ;
#4088 = ORIENTED_EDGE ( 'NONE', *, *, #865, .F. ) ;
#4089 = DIRECTION ( 'NONE',  ( 0.000000000000000000, 0.000000000000000000, 1.000000000000000000 ) ) ;
#4090 = SPHERICAL_SURFACE ( 'NONE', #4737, 3.000000000000000000 ) ;
#4091 = VERTEX_POINT ( 'NONE', #3559 ) ;
#4092 = CONTEXT_DEPENDENT_SHAPE_REPRESENTATION ( #2059, #3664 ) ;
#4093 = ADVANCED_BREP_SHAPE_REPRESENTATION ( '', ( #6277, #1914 ), #314 ) ;
#4094 = EDGE_CURVE ( 'NONE', #2768, #6974, #1704, .T. ) ;
#4095 = CARTESIAN_POINT ( 'NONE',  ( 201.3397459621555754, -3.000000000000000888, 39.99999999999997868 ) ) ;
#4096 = CARTESIAN_POINT ( 'NONE',  ( 200.0000000000000000, -11.00000000000000355, 8.660254037844387298 ) ) ;
#4097 = ORIENTED_EDGE ( 'NONE', *, *, #6201, .T. ) ;
#4098 = DIRECTION ( 'NONE',  ( 4.379057701015054125E-46, 0.2588190451025207950, 0.9659258262890683122 ) ) ;
#4099 = FACE_OUTER_BOUND ( 'NONE', #6647, .T. ) ;
#4100 = CARTESIAN_POINT ( 'NONE',  ( 30.00000000000000000, 0.000000000000000000, 8.000000000000003553 ) ) ;
#4101 = CARTESIAN_POINT ( 'NONE',  ( 217.0000000000000000, -1.445602896647342072E-15, 7.000000000000012434 ) ) ;
#4102 = EDGE_CURVE ( 'NONE', #7468, #4738, #4463, .T. ) ;
#4103 = CARTESIAN_POINT ( 'NONE',  ( 209.9999999999999716, 9.000000000000001776, 18.00000000000001066 ) ) ;
#4104 = CARTESIAN_POINT ( 'NONE',  ( -18.84314575050759188, 16.00000000000006395, 36.34314575050770202 ) ) ;
#4105 = EDGE_LOOP ( 'NONE', ( #2184, #3975, #2690, #2563, #6844, #2104, #6547, #5304, #3006, #3040, #4397, #3542 ) ) ;
#4106 = AXIS2_PLACEMENT_3D ( 'NONE', #2105, #951, #5150 ) ;
#4107 = ORIENTED_EDGE ( 'NONE', *, *, #5786, .T. ) ;
#4108 =( LENGTH_UNIT ( ) NAMED_UNIT ( * ) SI_UNIT ( .MILLI., .METRE. ) );
#4109 = FACE_OUTER_BOUND ( 'NONE', #3291, .T. ) ;
#4110 = CARTESIAN_POINT ( 'NONE',  ( -12.50000000000001066, -218.0630240738404950, 95.20959099461346398 ) ) ;
#4111 = DIRECTION ( 'NONE',  ( -0.000000000000000000, -1.000000000000000000, 0.000000000000000000 ) ) ;
#4112 = CARTESIAN_POINT ( 'NONE',  ( 170.0000000000000000, 11.00000000000000711, 8.660254037844383745 ) ) ;
#4113 = CONICAL_SURFACE ( 'NONE', #5083, 10.00000000000000355, 0.7853981633974500554 ) ;
#4114 = VECTOR ( 'NONE', #6300, 1000.000000000000000 ) ;
#4115 =( BOUNDED_SURFACE ( )  B_SPLINE_SURFACE ( 3, 2, ( 
 ( #477, #6374, #7399 ),
 ( #3454, #6248, #7365 ),
 ( #2098, #6905, #3332 ),
 ( #400, #5757, #6867 ),
 ( #2826, #5178, #2709 ),
 ( #5794, #1587, #4447 ),
 ( #3875, #7444, #3987 ),
 ( #516, #943, #1016 ),
 ( #445, #6791, #2256 ),
 ( #2133, #2177, #1511 ) ),
 .UNSPECIFIED., .F., .F., .T. ) 
 B_SPLINE_SURFACE_WITH_KNOTS ( ( 4, 2, 2, 2, 4 ),
 ( 3, 3 ),
 ( 1.570796326794896558, 1.965851602983812896, 2.360906879172729234, 2.755962155361645571, 3.151017431550562353 ),
 ( 0.000000000000000000, 1.000000000000000000 ),
 .UNSPECIFIED. ) 
 GEOMETRIC_REPRESENTATION_ITEM ( )  RATIONAL_B_SPLINE_SURFACE ( (
 ( 1.000000000000000000, 0.7071067811865475727, 1.000000000000000000),
 ( 1.000000000000000000, 0.7304008256110219310, 1.000000000000000000),
 ( 1.000000000000000000, 0.7524735362752019707, 1.000000000000000000),
 ( 1.000000000000000000, 0.7918254010917817887, 1.000000000000000000),
 ( 1.000000000000000000, 0.8090963605090051303, 1.000000000000000000),
 ( 1.000000000000000000, 0.8372423287799937164, 1.000000000000000000),
 ( 1.000000000000000000, 0.8481212422410200347, 1.000000000000000000),
 ( 1.000000000000000000, 0.8625983312438976203, 1.000000000000000000),
 ( 1.000000000000000000, 0.8662073891937924763, 1.000000000000000000),
 ( 1.000000000000000000, 0.8660189933120610029, 1.000000000000000000) ) ) 
 REPRESENTATION_ITEM ( '' )  SURFACE ( )  );
#4116 = ORIENTED_EDGE ( 'NONE', *, *, #5624, .F. ) ;
#4117 = EDGE_CURVE ( 'NONE', #5355, #868, #7406, .T. ) ;
#4118 = VERTEX_POINT ( 'NONE', #7094 ) ;
#4119 = VECTOR ( 'NONE', #1187, 1000.000000000000000 ) ;
#4120 = VECTOR ( 'NONE', #1863, 1000.000000000000000 ) ;
#4121 = AXIS2_PLACEMENT_3D ( 'NONE', #223, #4299, #6064 ) ;
#4122 = LINE ( 'NONE', #2380, #4769 ) ;
#4123 = CARTESIAN_POINT ( 'NONE',  ( 50.00000000000000000, 30.03170604878415162, 13.00000000000001066 ) ) ;
#4124 = ORIENTED_EDGE ( 'NONE', *, *, #4852, .F. ) ;
#4125 = CARTESIAN_POINT ( 'NONE',  ( -70.19709702122540307, -218.4687108041560180, 77.94269080187309839 ) ) ;
#4126 = DIRECTION ( 'NONE',  ( 5.605193857299270773E-45, 0.000000000000000000, 1.000000000000000000 ) ) ;
#4127 = DIRECTION ( 'NONE',  ( 5.551115123125782702E-17, 1.000000000000000000, 0.000000000000000000 ) ) ;
#4128 = ORIENTED_EDGE ( 'NONE', *, *, #656, .F. ) ;
#4129 = ORIENTED_EDGE ( 'NONE', *, *, #3338, .F. ) ;
#4130 = ORIENTED_EDGE ( 'NONE', *, *, #561, .F. ) ;
#4131 = LINE ( 'NONE', #5435, #6446 ) ;
#4132 = CARTESIAN_POINT ( 'NONE',  ( 10.29386626619291434, -219.0153713307822727, 95.37751551101595737 ) ) ;
#4133 = ORIENTED_EDGE ( 'NONE', *, *, #5871, .F. ) ;
#4134 = ITEM_DEFINED_TRANSFORMATION ( 'NONE', 'NONE', #2288,  #1914 ) ;
#4135 = CARTESIAN_POINT ( 'NONE',  ( 40.00000000000000000, -4.163336342344337027E-14, 1.387778780781445676E-14 ) ) ;
#4136 = DIRECTION ( 'NONE',  ( 0.000000000000000000, 0.000000000000000000, 1.000000000000000000 ) ) ;
#4137 = ORIENTED_EDGE ( 'NONE', *, *, #3200, .T. ) ;
#4138 = ADVANCED_FACE ( 'NONE', ( #2974 ), #4678, .F. ) ;
#4139 = EDGE_CURVE ( 'NONE', #3586, #6255, #3242, .T. ) ;
#4140 = CARTESIAN_POINT ( 'NONE',  ( -26.50000000000000355, -120.9522879036833558, 45.92078884797940219 ) ) ;
#4141 = CARTESIAN_POINT ( 'NONE',  ( -18.00000000000000000, 2.204364238465234639E-15, -39.99999999999997868 ) ) ;
#4142 = EDGE_LOOP ( 'NONE', ( #697, #5868, #4857, #3502, #2362, #2610, #278, #4060, #4782, #818, #2996, #5891, #2077, #5617, #1012, #1, #3706, #7185, #125, #5333 ) ) ;
#4143 = AXIS2_PLACEMENT_3D ( 'NONE', #759, #1990, #3185 ) ;
#4144 = CARTESIAN_POINT ( 'NONE',  ( -27.07790214619733860, -113.7796841263389069, 41.77968412633906325 ) ) ;
#4145 = CARTESIAN_POINT ( 'NONE',  ( 12.13610945967080923, -218.0630240738405519, 95.09600923956017482 ) ) ;
#4146 = CARTESIAN_POINT ( 'NONE',  ( 18.51125185374242932, -223.0630240738404950, 92.54436274715045840 ) ) ;
#4147 = CARTESIAN_POINT ( 'NONE',  ( 50.00000000000000000, 24.90486745229362953, 37.17889356869155648 ) ) ;
#4148 = AXIS2_PLACEMENT_3D ( 'NONE', #4190, #7177, #6494 ) ;
#4149 = ADVANCED_FACE ( 'NONE', ( #2400 ), #4759, .F. ) ;
#4150 = ORIENTED_EDGE ( 'NONE', *, *, #4194, .T. ) ;
#4151 = EDGE_CURVE ( 'NONE', #2347, #4912, #5201, .T. ) ;
#4152 = DIRECTION ( 'NONE',  ( 5.254869241218065572E-46, -0.7071067811865465735, 0.7071067811865485719 ) ) ;
#4153 = DIRECTION ( 'NONE',  ( -3.081487911019577365E-33, -1.193489751472043281E-15, 1.000000000000000000 ) ) ;
#4154 = DIRECTION ( 'NONE',  ( 0.000000000000000000, 0.000000000000000000, 1.000000000000000000 ) ) ;
#4155 = PRODUCT_DEFINITION ( 'UNKNOWN', '', #3393, #21 ) ;
#4156 = CARTESIAN_POINT ( 'NONE',  ( 50.00000000000000000, 0.000000000000000000, 35.00000000000000000 ) ) ;
#4157 = CARTESIAN_POINT ( 'NONE',  ( 187.7042917662940340, 7.845594361310616272, 15.00000000000000888 ) ) ;
#4158 = CARTESIAN_POINT ( 'NONE',  ( 189.5040654437683258, -6.000000000000000000, 19.50000000000000355 ) ) ;
#4159 = AXIS2_PLACEMENT_3D ( 'NONE', #3823, #6157, #2660 ) ;
#4160 = VERTEX_POINT ( 'NONE', #1934 ) ;
#4161 = ORIENTED_EDGE ( 'NONE', *, *, #4082, .T. ) ;
#4162 = DIRECTION ( 'NONE',  ( -1.000000000000000000, 0.000000000000000000, -7.663350976776343357E-46 ) ) ;
#4163 = LINE ( 'NONE', #5853, #2881 ) ;
#4164 = ORIENTED_EDGE ( 'NONE', *, *, #983, .T. ) ;
#4165 = CARTESIAN_POINT ( 'NONE',  ( -60.83909347413334245, -228.8136496942593112, 74.82215363428544208 ) ) ;
#4166 = CARTESIAN_POINT ( 'NONE',  ( 46.99999999999999289, -25.88825784476432545, 10.00000000000000533 ) ) ;
#4167 = DIRECTION ( 'NONE',  ( 1.000000000000000000, 0.000000000000000000, 0.000000000000000000 ) ) ;
#4168 = ORIENTED_EDGE ( 'NONE', *, *, #7107, .F. ) ;
#4169 = EDGE_LOOP ( 'NONE', ( #1952, #2157, #4483, #6885 ) ) ;
#4170 = CARTESIAN_POINT ( 'NONE',  ( 48.75735931288071612, -25.78715168812825809, 12.89530150989249258 ) ) ;
#4171 = CARTESIAN_POINT ( 'NONE',  ( 17.73846410710429211, -217.2436419687045657, 95.06511182196470600 ) ) ;
#4172 = ORIENTED_EDGE ( 'NONE', *, *, #5713, .F. ) ;
#4173 = SHAPE_DEFINITION_REPRESENTATION ( #7078, #7252 ) ;
#4174 = EDGE_CURVE ( 'NONE', #2464, #7550, #2408, .T. ) ;
#4175 = FACE_OUTER_BOUND ( 'NONE', #650, .T. ) ;
#4176 = ADVANCED_FACE ( 'NONE', ( #6123 ), #2044, .T. ) ;
#4177 = DIRECTION ( 'NONE',  ( 0.000000000000000000, -1.000000000000000000, 0.000000000000000000 ) ) ;
#4178 = ORIENTED_EDGE ( 'NONE', *, *, #4709, .T. ) ;
#4179 = FACE_OUTER_BOUND ( 'NONE', #4847, .T. ) ;
#4180 = CARTESIAN_POINT ( 'NONE',  ( 25.00000000000000711, 40.21320343559642652, 0.9999999999999956701 ) ) ;
#4181 = ORIENTED_EDGE ( 'NONE', *, *, #4532, .F. ) ;
#4182 =( REPRESENTATION_RELATIONSHIP ('NONE','NONE', #4862, #867 ) REPRESENTATION_RELATIONSHIP_WITH_TRANSFORMATION ( #2897 )SHAPE_REPRESENTATION_RELATIONSHIP( ) );
#4183 = ADVANCED_FACE ( 'NONE', ( #6702 ), #6626, .T. ) ;
#4184 = CARTESIAN_POINT ( 'NONE',  ( 13.93877027101358124, -218.0630240738406087, 94.58489134182006808 ) ) ;
#4185 = FACE_OUTER_BOUND ( 'NONE', #1183, .T. ) ;
#4186 = DIRECTION ( 'NONE',  ( 0.000000000000000000, 0.000000000000000000, -1.000000000000000000 ) ) ;
#4187 = PRODUCT_DEFINITION_CONTEXT ( 'detailed design', #3238, 'design' ) ;
#4188 = AXIS2_PLACEMENT_3D ( 'NONE', #781, #3759, #3647 ) ;
#4189 = VECTOR ( 'NONE', #5292, 1000.000000000000000 ) ;
#4190 = CARTESIAN_POINT ( 'NONE',  ( 0.000000000000000000, 0.000000000000000000, -9.999999999999994671 ) ) ;
#4191 = CARTESIAN_POINT ( 'NONE',  ( 0.000000000000000000, -28.78532416918554304, 7.000000000000006217 ) ) ;
#4192 = CARTESIAN_POINT ( 'NONE',  ( -23.84314575050761320, 16.00000000000004619, 36.65685424949246851 ) ) ;
#4193 = CARTESIAN_POINT ( 'NONE',  ( 209.9999999999999716, -6.000000000000000000, 28.99999999999998579 ) ) ;
#4194 = EDGE_CURVE ( 'NONE', #7551, #6429, #1785, .T. ) ;
#4195 = ORIENTED_EDGE ( 'NONE', *, *, #3570, .T. ) ;
#4196 = ORIENTED_EDGE ( 'NONE', *, *, #5004, .F. ) ;
#4197 = CIRCLE ( 'NONE', #1605, 6.000000000000000000 ) ;
#4198 = CARTESIAN_POINT ( 'NONE',  ( 53.00000000000000000, -26.29852790585433198, 10.00000000000000888 ) ) ;
#4199 = DIRECTION ( 'NONE',  ( 1.000000000000000000, 2.465190328815661892E-32, -9.244463733058732095E-33 ) ) ;
#4200 = EDGE_LOOP ( 'NONE', ( #5919, #3909, #2110, #2351, #3276 ) ) ;
#4201 = CARTESIAN_POINT ( 'NONE',  ( -60.66745985056476798, -217.4114710059388926, 71.76694906279429631 ) ) ;
#4202 = CARTESIAN_POINT ( 'NONE',  ( 48.57048730951588311, -28.62906503896529031, 10.00000000000000533 ) ) ;
#4203 = ADVANCED_FACE ( 'NONE', ( #6737 ), #1967, .T. ) ;
#4204 = CARTESIAN_POINT ( 'NONE',  ( -62.83175576870043955, -218.0623705734561497, 89.75267118170498293 ) ) ;
#4205 = MECHANICAL_DESIGN_GEOMETRIC_PRESENTATION_REPRESENTATION (  '', ( #7145 ), #4514 ) ;
#4206 = ORIENTED_EDGE ( 'NONE', *, *, #7514, .F. ) ;
#4207 = ORIENTED_EDGE ( 'NONE', *, *, #7545, .T. ) ;
#4208 = CARTESIAN_POINT ( 'NONE',  ( 25.00000000000002132, 0.000000000000000000, 4.999999999999992006 ) ) ;
#4209 = CARTESIAN_POINT ( 'NONE',  ( 27.08493024494318746, -223.4607234779399789, 79.16428349862680136 ) ) ;
#4210 = ORIENTED_EDGE ( 'NONE', *, *, #3493, .T. ) ;
#4211 = DIRECTION ( 'NONE',  ( 1.000000000000000000, 0.000000000000000000, 0.000000000000000000 ) ) ;
#4212 = DIRECTION ( 'NONE',  ( 0.000000000000000000, 0.000000000000000000, -1.000000000000000000 ) ) ;
#4213 = CIRCLE ( 'NONE', #5313, 6.000000000000000000 ) ;
#4214 = ORIENTED_EDGE ( 'NONE', *, *, #3585, .T. ) ;
#4215 = ADVANCED_FACE ( 'NONE', ( #7204, #5440, #2471 ), #4828, .F. ) ;
#4216 = ADVANCED_FACE ( 'NONE', ( #3709 ), #5402, .F. ) ;
#4217 = FACE_OUTER_BOUND ( 'NONE', #4169, .T. ) ;
#4218 = CARTESIAN_POINT ( 'NONE',  ( 185.0000000000000000, -39.99999999999999289, 0.000000000000000000 ) ) ;
#4219 = LINE ( 'NONE', #5255, #3017 ) ;
#4220 = CARTESIAN_POINT ( 'NONE',  ( 14.29503225977587633, -218.0630240738405803, 94.45153243777278362 ) ) ;
#4221 = DIRECTION ( 'NONE',  ( -0.000000000000000000, -0.000000000000000000, 1.000000000000000000 ) ) ;
#4222 = CYLINDRICAL_SURFACE ( 'NONE', #1428, 2.999999999999999112 ) ;
#4223 =( NAMED_UNIT ( * ) SI_UNIT ( $, .STERADIAN. ) SOLID_ANGLE_UNIT ( ) );
#4224 = CARTESIAN_POINT ( 'NONE',  ( 48.96690339724148799, 26.58792303940015600, 10.00000000000068745 ) ) ;
#4225 = CYLINDRICAL_SURFACE ( 'NONE', #4702, 8.000000000000028422 ) ;
#4226 = CARTESIAN_POINT ( 'NONE',  ( 50.00000000000000000, -21.98659819442010388, 35.76778892745510063 ) ) ;
#4227 = CARTESIAN_POINT ( 'NONE',  ( 10.32550510630198737, -219.7296907405018089, 95.50346929579330890 ) ) ;
#4228 = CARTESIAN_POINT ( 'NONE',  ( -21.50000000000000000, -215.0630240738404950, 94.68061005248806339 ) ) ;
#4229 = AXIS2_PLACEMENT_3D ( 'NONE', #4798, #7557, #3528 ) ;
#4230 = ORIENTED_EDGE ( 'NONE', *, *, #5643, .F. ) ;
#4231 = EDGE_LOOP ( 'NONE', ( #2123, #1505 ) ) ;
#4232 = EDGE_CURVE ( 'NONE', #5048, #3850, #1383, .T. ) ;
#4233 = DIRECTION ( 'NONE',  ( -1.000000000000000000, -2.465190328815661892E-32, -9.244463733058733463E-33 ) ) ;
#4234 = VECTOR ( 'NONE', #3825, 1000.000000000000000 ) ;
#4235 = CARTESIAN_POINT ( 'NONE',  ( -53.25562355766777500, -218.1519544391844079, 95.22527181742783853 ) ) ;
#4236 = CIRCLE ( 'NONE', #3750, 14.00000000000000711 ) ;
#4237 = CARTESIAN_POINT ( 'NONE',  ( -60.75121803101544060, -222.9757987891385369, 73.25790619872466891 ) ) ;
#4238 = LINE ( 'NONE', #6583, #870 ) ;
#4239 = CARTESIAN_POINT ( 'NONE',  ( -54.71793473364260052, -218.0620782339077834, 95.13813623280537968 ) ) ;
#4240 = ORIENTED_EDGE ( 'NONE', *, *, #911, .T. ) ;
#4241 = AXIS2_PLACEMENT_3D ( 'NONE', #2193, #4046, #5237 ) ;
#4242 = VECTOR ( 'NONE', #6865, 1000.000000000000000 ) ;
#4243 = AXIS2_PLACEMENT_3D ( 'NONE', #2697, #320, #7388 ) ;
#4244 = VERTEX_POINT ( 'NONE', #240 ) ;
#4245 = EDGE_CURVE ( 'NONE', #6726, #7349, #4469, .T. ) ;
#4246 = DIRECTION ( 'NONE',  ( 1.000000000000000000, 0.000000000000000000, 0.000000000000000000 ) ) ;
#4247 = CARTESIAN_POINT ( 'NONE',  ( 27.12218822116579631, -221.8025471834170048, 78.75851208262513126 ) ) ;
#4248 = EDGE_LOOP ( 'NONE', ( #6659, #2567, #7535, #2543 ) ) ;
#4249 = EDGE_CURVE ( 'NONE', #877, #1926, #167, .T. ) ;
#4250 = CONTEXT_DEPENDENT_SHAPE_REPRESENTATION ( #2208, #2318 ) ;
#4251 = AXIS2_PLACEMENT_3D ( 'NONE', #6232, #7499, #1040 ) ;
#4252 = PLANE ( 'NONE',  #138 ) ;
#4253 = CARTESIAN_POINT ( 'NONE',  ( -32.50000000000001421, -106.6736682753135739, 34.67366827531368756 ) ) ;
#4254 = ORIENTED_EDGE ( 'NONE', *, *, #7454, .T. ) ;
#4255 = CARTESIAN_POINT ( 'NONE',  ( 26.00000000000000000, 0.000000000000000000, 0.000000000000000000 ) ) ;
#4256 = CARTESIAN_POINT ( 'NONE',  ( -29.50000000000000000, -223.0630240738404950, 73.28127814332044920 ) ) ;
#4257 = ORIENTED_EDGE ( 'NONE', *, *, #4624, .T. ) ;
#4258 = CARTESIAN_POINT ( 'NONE',  ( 200.0000000000000000, -10.56957438397690829, -9.180637088000986878 ) ) ;
#4259 = CYLINDRICAL_SURFACE ( 'NONE', #7013, 17.99999999999999645 ) ;
#4260 = DIRECTION ( 'NONE',  ( -1.000000000000000000, 0.000000000000000000, 0.000000000000000000 ) ) ;
#4261 = ORIENTED_EDGE ( 'NONE', *, *, #3005, .F. ) ;
#4262 = CARTESIAN_POINT ( 'NONE',  ( -26.50000000000003197, 0.000000000000000000, 0.000000000000000000 ) ) ;
#4263 = FACE_OUTER_BOUND ( 'NONE', #2850, .T. ) ;
#4264 = CARTESIAN_POINT ( 'NONE',  ( 3.000000000000002665, 30.03170604878415162, 7.000000000000012434 ) ) ;
#4265 = CARTESIAN_POINT ( 'NONE',  ( -60.94741519416551512, -223.0630598631611861, 76.40853535907753269 ) ) ;
#4266 = CARTESIAN_POINT ( 'NONE',  ( 191.1954203846383393, -6.078081970536771017, 17.21475634561434731 ) ) ;
#4267 = EDGE_CURVE ( 'NONE', #1052, #2698, #7310, .T. ) ;
#4268 = AXIS2_PLACEMENT_3D ( 'NONE', #4892, #7306, #3188 ) ;
#4269 = ORIENTED_EDGE ( 'NONE', *, *, #3084, .T. ) ;
#4270 = ORIENTED_EDGE ( 'NONE', *, *, #4361, .F. ) ;
#4271 = LINE ( 'NONE', #4780, #3030 ) ;
#4272 = AXIS2_PLACEMENT_3D ( 'NONE', #2176, #2211, #6902 ) ;
#4273 = LINE ( 'NONE', #2494, #4119 ) ;
#4274 = CARTESIAN_POINT ( 'NONE',  ( -70.24145449743711822, -216.4945693450226543, 77.45959972289216466 ) ) ;
#4275 = EDGE_CURVE ( 'NONE', #1071, #5437, #421, .T. ) ;
#4276 = CARTESIAN_POINT ( 'NONE',  ( -22.32280336819470890, -65.17719663180518808, 38.17719663180528045 ) ) ;
#4277 = CARTESIAN_POINT ( 'NONE',  ( -64.38803740020385646, -218.0613621616423927, 85.37521886293086482 ) ) ;
#4278 = ORIENTED_EDGE ( 'NONE', *, *, #5690, .T. ) ;
#4279 = ORIENTED_EDGE ( 'NONE', *, *, #2696, .F. ) ;
#4280 = DIRECTION ( 'NONE',  ( -5.254869241218064794E-46, 0.7071067811865464625, -0.7071067811865485719 ) ) ;
#4281 = CARTESIAN_POINT ( 'NONE',  ( 17.66255603274094454, -217.0856944719845103, 71.67965750360849597 ) ) ;
#4282 = VERTEX_POINT ( 'NONE', #6012 ) ;
#4283 = DIRECTION ( 'NONE',  ( 0.000000000000000000, 0.000000000000000000, -1.000000000000000000 ) ) ;
#4284 = DIRECTION ( 'NONE',  ( 0.000000000000000000, 0.000000000000000000, -1.000000000000000000 ) ) ;
#4285 = ADVANCED_FACE ( 'NONE', ( #7164 ), #6593, .F. ) ;
#4286 = EDGE_CURVE ( 'NONE', #4738, #131, #2811, .T. ) ;
#4287 = ORIENTED_EDGE ( 'NONE', *, *, #833, .F. ) ;
#4288 = LINE ( 'NONE', #1787, #824 ) ;
#4289 = CARTESIAN_POINT ( 'NONE',  ( 4.000000000000000000, -2.887003712633254693E-29, 6.000000000000000888 ) ) ;
#4290 = EDGE_LOOP ( 'NONE', ( #7028, #5114, #1001, #2705 ) ) ;
#4291 =( NAMED_UNIT ( * ) SI_UNIT ( $, .STERADIAN. ) SOLID_ANGLE_UNIT ( ) );
#4292 = CARTESIAN_POINT ( 'NONE',  ( -32.50000000000001421, -99.90626354475344328, 72.90626354475362803 ) ) ;
#4293 = CYLINDRICAL_SURFACE ( 'NONE', #1225, 8.500000000000007105 ) ;
#4294 = DIRECTION ( 'NONE',  ( 0.000000000000000000, -0.03489949670250429292, -0.9993908270190955401 ) ) ;
#4295 = EDGE_CURVE ( 'NONE', #6417, #5692, #6271, .T. ) ;
#4296 = ORIENTED_EDGE ( 'NONE', *, *, #449, .F. ) ;
#4297 = CARTESIAN_POINT ( 'NONE',  ( 185.0000000000000000, -39.99999999999999289, 10.00000000000000355 ) ) ;
#4298 = DIRECTION ( 'NONE',  ( -5.551115123125785167E-17, 0.7071067811865452413, -0.7071067811865499042 ) ) ;
#4299 = DIRECTION ( 'NONE',  ( -4.237045877651920929E-33, -2.600005424922769496E-32, 1.000000000000000000 ) ) ;
#4300 = CARTESIAN_POINT ( 'NONE',  ( -63.74607179430710602, -223.0630176522924444, 88.91434613420386768 ) ) ;
#4301 = DIRECTION ( 'NONE',  ( 4.622231866529368100E-33, -2.600005424922769496E-32, 1.000000000000000000 ) ) ;
#4302 = AXIS2_PLACEMENT_3D ( 'NONE', #2331, #5376, #2982 ) ;
#4303 = EDGE_LOOP ( 'NONE', ( #397, #1668, #3692, #6284 ) ) ;
#4304 = ORIENTED_EDGE ( 'NONE', *, *, #1053, .F. ) ;
#4305 = EDGE_CURVE ( 'NONE', #6424, #1438, #5478, .T. ) ;
#4306 = DIRECTION ( 'NONE',  ( 0.000000000000000000, 0.000000000000000000, -1.000000000000000000 ) ) ;
#4307 = CARTESIAN_POINT ( 'NONE',  ( -22.45815546247371586, -110.0418445375260603, 38.04184453752623796 ) ) ;
#4308 = CIRCLE ( 'NONE', #1348, 6.000000000000019540 ) ;
#4309 = CIRCLE ( 'NONE', #1721, 3.000000000000000000 ) ;
#4310 = DIRECTION ( 'NONE',  ( 1.000000000000000000, 0.000000000000000000, 0.000000000000000000 ) ) ;
#4311 = CARTESIAN_POINT ( 'NONE',  ( -61.28154286849950694, -218.0630231266628698, 91.76994857279252926 ) ) ;
#4312 = VERTEX_POINT ( 'NONE', #3400 ) ;
#4313 = VECTOR ( 'NONE', #4677, 1000.000000000000000 ) ;
#4314 = ORIENTED_EDGE ( 'NONE', *, *, #5268, .F. ) ;
#4315 = EDGE_CURVE ( 'NONE', #7201, #3547, #2118, .T. ) ;
#4316 = FACE_OUTER_BOUND ( 'NONE', #4946, .T. ) ;
#4317 = CARTESIAN_POINT ( 'NONE',  ( 200.0000000000000000, -11.00000000000000355, 8.660254037844387298 ) ) ;
#4318 = ORIENTED_EDGE ( 'NONE', *, *, #3439, .T. ) ;
#4319 = VECTOR ( 'NONE', #5697, 1000.000000000000000 ) ;
#4320 = CARTESIAN_POINT ( 'NONE',  ( -16.49999999999996447, 0.000000000000000000, 0.000000000000000000 ) ) ;
#4321 = CARTESIAN_POINT ( 'NONE',  ( 217.0000000000000000, 56.99999999999999289, 0.000000000000000000 ) ) ;
#4322 = VERTEX_POINT ( 'NONE', #4588 ) ;
#4323 = CARTESIAN_POINT ( 'NONE',  ( -13.50000000000000355, 16.00000000000003553, 42.31370849898485886 ) ) ;
#4324 = EDGE_CURVE ( 'NONE', #2040, #4037, #1415, .T. ) ;
#4325 = LINE ( 'NONE', #281, #4480 ) ;
#4326 = VERTEX_POINT ( 'NONE', #5623 ) ;
#4327 = CIRCLE ( 'NONE', #6154, 9.999999999999998224 ) ;
#4328 = CARTESIAN_POINT ( 'NONE',  ( 1.387778780781445676E-14, 12.49999999999998401, 4.999999999999999112 ) ) ;
#4329 = LINE ( 'NONE', #1393, #4808 ) ;
#4330 = FACE_OUTER_BOUND ( 'NONE', #1193, .T. ) ;
#4331 = ORIENTED_EDGE ( 'NONE', *, *, #5136, .T. ) ;
#4332 = AXIS2_PLACEMENT_3D ( 'NONE', #5559, #1356, #2478 ) ;
#4333 = DIRECTION ( 'NONE',  ( 0.000000000000000000, 1.000000000000000000, 0.000000000000000000 ) ) ;
#4334 = EDGE_CURVE ( 'NONE', #228, #5778, #3774, .T. ) ;
#4335 = FACE_OUTER_BOUND ( 'NONE', #7396, .T. ) ;
#4336 = FACE_OUTER_BOUND ( 'NONE', #783, .T. ) ;
#4337 = CARTESIAN_POINT ( 'NONE',  ( 4.000000000000003553, 0.000000000000000000, 6.000000000000015099 ) ) ;
#4338 = CARTESIAN_POINT ( 'NONE',  ( -63.80434472310041372, -223.0629276316900018, 88.75851834311229993 ) ) ;
#4339 = EDGE_LOOP ( 'NONE', ( #3189, #380, #1548, #1743 ) ) ;
#4340 = FACE_OUTER_BOUND ( 'NONE', #3122, .T. ) ;
#4341 = ADVANCED_FACE ( 'NONE', ( #960 ), #1000, .T. ) ;
#4342 = ORIENTED_EDGE ( 'NONE', *, *, #1625, .T. ) ;
#4343 = VECTOR ( 'NONE', #3598, 1000.000000000000000 ) ;
#4344 = VERTEX_POINT ( 'NONE', #4467 ) ;
#4345 = DIRECTION ( 'NONE',  ( -7.623657272262518365E-17, -0.7071067811865464625, 0.7071067811865486830 ) ) ;
#4346 = CARTESIAN_POINT ( 'NONE',  ( 0.000000000000000000, 0.000000000000000000, -39.99999999999997868 ) ) ;
#4347 = DIRECTION ( 'NONE',  ( 0.000000000000000000, -1.000000000000000000, -1.221245327087672392E-15 ) ) ;
#4348 = AXIS2_PLACEMENT_3D ( 'NONE', #2990, #7032, #74 ) ;
#4349 = CYLINDRICAL_SURFACE ( 'NONE', #3761, 3.000000000000002665 ) ;
#4350 = EDGE_CURVE ( 'NONE', #3892, #1997, #5110, .T. ) ;
#4351 = ORIENTED_EDGE ( 'NONE', *, *, #80, .T. ) ;
#4352 = ORIENTED_EDGE ( 'NONE', *, *, #4315, .F. ) ;
#4353 = VECTOR ( 'NONE', #6148, 1000.000000000000000 ) ;
#4354 = VECTOR ( 'NONE', #5267, 1000.000000000000000 ) ;
#4355 = DIRECTION ( 'NONE',  ( 1.000000000000000000, -0.000000000000000000, -0.000000000000000000 ) ) ;
#4356 = CARTESIAN_POINT ( 'NONE',  ( 17.70193531918452123, -219.7017882839736274, 72.38063772785838523 ) ) ;
#4357 = EDGE_LOOP ( 'NONE', ( #662, #5524, #1044, #423 ) ) ;
#4358 = FACE_OUTER_BOUND ( 'NONE', #534, .T. ) ;
#4359 = DIRECTION ( 'NONE',  ( -1.000000000000000000, -0.000000000000000000, -0.000000000000000000 ) ) ;
#4360 = AXIS2_PLACEMENT_3D ( 'NONE', #6267, #5078, #6310 ) ;
#4361 = EDGE_CURVE ( 'NONE', #2111, #3994, #4549, .T. ) ;
#4362 = PRESENTATION_LAYER_ASSIGNMENT (  '', '', ( #5582 ) ) ;
#4363 = VECTOR ( 'NONE', #1026, 1000.000000000000114 ) ;
#4364 =( BOUNDED_CURVE ( )  B_SPLINE_CURVE ( 3, ( #6219, #2834, #5034, #6875 ),
 .UNSPECIFIED., .F., .T. ) 
 B_SPLINE_CURVE_WITH_KNOTS ( ( 4, 4 ),
 ( 1.570796326794896558, 3.141592653589793116 ),
 .UNSPECIFIED. ) 
 CURVE ( )  GEOMETRIC_REPRESENTATION_ITEM ( )  RATIONAL_B_SPLINE_CURVE ( ( 1.000000000000000000, 0.8047378541243649375, 0.8047378541243649375, 1.000000000000000000 ) ) 
 REPRESENTATION_ITEM ( '' )  );
#4365 = ORIENTED_EDGE ( 'NONE', *, *, #6538, .T. ) ;
#4366 = LINE ( 'NONE', #7278, #220 ) ;
#4367 = VECTOR ( 'NONE', #953, 999.9999999999998863 ) ;
#4368 = CIRCLE ( 'NONE', #2882, 17.99999999999999645 ) ;
#4369 = CARTESIAN_POINT ( 'NONE',  ( 49.98952410273115987, 24.81497846033548527, 10.00000000000000178 ) ) ;
#4370 = FACE_OUTER_BOUND ( 'NONE', #7231, .T. ) ;
#4371 = AXIS2_PLACEMENT_3D ( 'NONE', #6211, #7516, #2864 ) ;
#4372 = ORIENTED_EDGE ( 'NONE', *, *, #4471, .T. ) ;
#4373 = CARTESIAN_POINT ( 'NONE',  ( -29.35769912250765046, -110.6367035073516831, 38.63670350735182524 ) ) ;
#4374 = DIRECTION ( 'NONE',  ( 0.000000000000000000, 1.301042606982602954E-15, -1.000000000000000000 ) ) ;
#4375 = DIRECTION ( 'NONE',  ( -0.000000000000000000, -1.000000000000000000, -0.000000000000000000 ) ) ;
#4376 = ADVANCED_FACE ( 'NONE', ( #464 ), #6928, .F. ) ;
#4377 = EDGE_CURVE ( 'NONE', #3, #6696, #6462, .T. ) ;
#4378 = VERTEX_POINT ( 'NONE', #7384 ) ;
#4379 = DIRECTION ( 'NONE',  ( 1.000000000000000000, 2.465190328815661892E-32, -9.244463733058732095E-33 ) ) ;
#4380 = CARTESIAN_POINT ( 'NONE',  ( 6.938893903907228378E-15, 73.78679656440351664, 0.9999999999999991118 ) ) ;
#4381 = PLANE ( 'NONE',  #3756 ) ;
#4382 = CARTESIAN_POINT ( 'NONE',  ( -61.12936385255436988, -223.0630265135370109, 76.58851298612765390 ) ) ;
#4383 = LINE ( 'NONE', #2065, #6266 ) ;
#4384 = EDGE_CURVE ( 'NONE', #4660, #245, #3237, .T. ) ;
#4385 = ADVANCED_FACE ( 'NONE', ( #315 ), #5081, .F. ) ;
#4386 = ORIENTED_EDGE ( 'NONE', *, *, #2526, .F. ) ;
#4387 = AXIS2_PLACEMENT_3D ( 'NONE', #6382, #3461, #4154 ) ;
#4388 = ORIENTED_EDGE ( 'NONE', *, *, #3226, .F. ) ;
#4389 = DIRECTION ( 'NONE',  ( -2.465190328815661892E-32, -1.000000000000000000, -1.193489751472043281E-15 ) ) ;
#4390 = DIRECTION ( 'NONE',  ( -0.000000000000000000, 1.000000000000000000, 0.000000000000000000 ) ) ;
#4391 = CARTESIAN_POINT ( 'NONE',  ( 25.00000000000001421, 35.07106781186547551, 2.928932188134525827 ) ) ;
#4392 = VECTOR ( 'NONE', #4379, 1000.000000000000000 ) ;
#4393 = ORIENTED_EDGE ( 'NONE', *, *, #3368, .T. ) ;
#4394 = ORIENTED_EDGE ( 'NONE', *, *, #4709, .F. ) ;
#4395 = CIRCLE ( 'NONE', #3166, 6.000000000000000888 ) ;
#4396 = CARTESIAN_POINT ( 'NONE',  ( -16.50000000000000000, -214.0630240738404382, 70.86973541144034527 ) ) ;
#4397 = ORIENTED_EDGE ( 'NONE', *, *, #5076, .T. ) ;
#4398 = LINE ( 'NONE', #5658, #5663 ) ;
#4399 = DIRECTION ( 'NONE',  ( 0.000000000000000000, 0.000000000000000000, 1.000000000000000000 ) ) ;
#4400 = EDGE_LOOP ( 'NONE', ( #3302, #5040, #6186, #4254 ) ) ;
#4401 = DIRECTION ( 'NONE',  ( -1.000000000000000000, -1.725633230170963324E-31, 1.078147950931789387E-16 ) ) ;
#4402 = ADVANCED_FACE ( 'NONE', ( #1493 ), #1535, .F. ) ;
#4403 = CARTESIAN_POINT ( 'NONE',  ( 47.42432064489011623, 27.28271252672780989, 10.00000000000750155 ) ) ;
#4404 = CARTESIAN_POINT ( 'NONE',  ( 202.0000000000000568, -10.62218397927710356, -7.000000000000018652 ) ) ;
#4405 = ORIENTED_EDGE ( 'NONE', *, *, #682, .T. ) ;
#4406 = FACE_OUTER_BOUND ( 'NONE', #1581, .T. ) ;
#4407 = DIRECTION ( 'NONE',  ( -0.000000000000000000, 1.000000000000000000, -0.000000000000000000 ) ) ;
#4408 = FACE_OUTER_BOUND ( 'NONE', #501, .T. ) ;
#4409 = EDGE_LOOP ( 'NONE', ( #5711, #6646, #2224, #6835 ) ) ;
#4410 = CARTESIAN_POINT ( 'NONE',  ( 220.0000000000000000, 60.00000000000000000, 3.000000000000021760 ) ) ;
#4411 = EDGE_CURVE ( 'NONE', #6942, #5661, #5397, .T. ) ;
#4412 =( NAMED_UNIT ( * ) SI_UNIT ( $, .STERADIAN. ) SOLID_ANGLE_UNIT ( ) );
#4413 = FACE_OUTER_BOUND ( 'NONE', #1108, .T. ) ;
#4414 = CARTESIAN_POINT ( 'NONE',  ( 220.0000000000000000, -3.000000000000000000, 18.00000000000001066 ) ) ;
#4415 = VERTEX_POINT ( 'NONE', #2196 ) ;
#4416 = LINE ( 'NONE', #3841, #2953 ) ;
#4417 = ORIENTED_EDGE ( 'NONE', *, *, #3130, .T. ) ;
#4418 = EDGE_LOOP ( 'NONE', ( #721, #2548, #4778, #7407 ) ) ;
#4419 = DIRECTION ( 'NONE',  ( 0.000000000000000000, 0.000000000000000000, -1.000000000000000000 ) ) ;
#4420 = DIRECTION ( 'NONE',  ( 6.162975822039156098E-33, 0.2588190451025209060, 0.9659258262890683122 ) ) ;
#4421 = EDGE_CURVE ( 'NONE', #6577, #2624, #1610, .T. ) ;
#4422 = CARTESIAN_POINT ( 'NONE',  ( 53.00000000000000711, 20.99999999999999645, 10.00000000000001066 ) ) ;
#4423 = VECTOR ( 'NONE', #3336, 1000.000000000000000 ) ;
#4424 = EDGE_LOOP ( 'NONE', ( #4020, #4438, #5775, #619 ) ) ;
#4425 = EDGE_LOOP ( 'NONE', ( #211, #3882, #6932, #6473 ) ) ;
#4426 = AXIS2_PLACEMENT_3D ( 'NONE', #402, #2748, #7446 ) ;
#4427 = VECTOR ( 'NONE', #4294, 1000.000000000000114 ) ;
#4428 = CARTESIAN_POINT ( 'NONE',  ( -12.50000000000000355, -218.0630240738404382, 71.94153218116483117 ) ) ;
#4429 = EDGE_CURVE ( 'NONE', #5303, #6262, #5458, .T. ) ;
#4430 = ORIENTED_EDGE ( 'NONE', *, *, #6132, .F. ) ;
#4431 = CARTESIAN_POINT ( 'NONE',  ( 1.387778780781445676E-14, 31.53553390593269512, 6.464466094067257806 ) ) ;
#4432 = DIRECTION ( 'NONE',  ( 0.7071067811865461294, 8.659560562355135004E-17, 0.7071067811865489050 ) ) ;
#4433 = AXIS2_PLACEMENT_3D ( 'NONE', #2981, #2522, #4875 ) ;
#4434 = ORIENTED_EDGE ( 'NONE', *, *, #2440, .F. ) ;
#4435 = LINE ( 'NONE', #1386, #2182 ) ;
#4436 = DIRECTION ( 'NONE',  ( -2.465190328815661892E-32, -1.000000000000000000, -1.193489751472043281E-15 ) ) ;
#4437 = FACE_OUTER_BOUND ( 'NONE', #1659, .T. ) ;
#4438 = ORIENTED_EDGE ( 'NONE', *, *, #5015, .F. ) ;
#4439 =( NAMED_UNIT ( * ) SI_UNIT ( $, .STERADIAN. ) SOLID_ANGLE_UNIT ( ) );
#4440 = CARTESIAN_POINT ( 'NONE',  ( -60.77671317003687790, -219.8343230396697834, 95.52191879319202883 ) ) ;
#4441 = DIRECTION ( 'NONE',  ( 0.000000000000000000, 0.000000000000000000, 1.000000000000000000 ) ) ;
#4442 = CARTESIAN_POINT ( 'NONE',  ( -26.50000000000003197, -49.37258300203047412, -6.000000000000002665 ) ) ;
#4443 = VERTEX_POINT ( 'NONE', #2925 ) ;
#4444 = EDGE_CURVE ( 'NONE', #4091, #6696, #5777, .T. ) ;
#4445 = ORIENTED_EDGE ( 'NONE', *, *, #3108, .F. ) ;
#4446 = CYLINDRICAL_SURFACE ( 'NONE', #90, 3.000000000000001332 ) ;
#4447 = CARTESIAN_POINT ( 'NONE',  ( 186.7220223217026671, 5.338718410048599594, 14.68135996373468899 ) ) ;
#4448 = CARTESIAN_POINT ( 'NONE',  ( -54.91295168136564797, -223.0620909472820586, 96.02094539123626760 ) ) ;
#4449 = CYLINDRICAL_SURFACE ( 'NONE', #7003, 13.99999999999999112 ) ;
#4450 = DIRECTION ( 'NONE',  ( -0.5773502691896309491, 0.5773502691896222894, -0.5773502691896239547 ) ) ;
#4451 = VECTOR ( 'NONE', #1029, 1000.000000000000000 ) ;
#4452 = EDGE_CURVE ( 'NONE', #4834, #1465, #3139, .T. ) ;
#4453 = VERTEX_POINT ( 'NONE', #3470 ) ;
#4454 = EDGE_LOOP ( 'NONE', ( #7075, #5564, #6474, #3508 ) ) ;
#4455 = CARTESIAN_POINT ( 'NONE',  ( 40.00000000000000000, -4.163336342344337027E-14, 8.000000000000000000 ) ) ;
#4456 = CARTESIAN_POINT ( 'NONE',  ( -32.50000000000002842, 6.938893903907228378E-15, 6.000000000000000000 ) ) ;
#4457 = CARTESIAN_POINT ( 'NONE',  ( 0.000000000000000000, -56.99999999999999289, 3.000000000000000444 ) ) ;
#4458 = DIRECTION ( 'NONE',  ( 0.000000000000000000, 0.000000000000000000, 1.000000000000000000 ) ) ;
#4459 = ADVANCED_FACE ( 'NONE', ( #5277 ), #1730, .T. ) ;
#4460 = ORIENTED_EDGE ( 'NONE', *, *, #1037, .T. ) ;
#4461 = EDGE_CURVE ( 'NONE', #5858, #3340, #4086, .T. ) ;
#4462 = ORIENTED_EDGE ( 'NONE', *, *, #5880, .F. ) ;
#4463 = CIRCLE ( 'NONE', #6434, 3.000000000000000000 ) ;
#4464 = DIRECTION ( 'NONE',  ( 0.000000000000000000, 0.000000000000000000, -1.000000000000000000 ) ) ;
#4465 = EDGE_LOOP ( 'NONE', ( #6297, #6117, #6704, #3383 ) ) ;
#4466 = LINE ( 'NONE', #276, #6530 ) ;
#4467 = CARTESIAN_POINT ( 'NONE',  ( -12.50000000000001066, -218.0630240738404950, 95.20959099461346398 ) ) ;
#4468 = ORIENTED_EDGE ( 'NONE', *, *, #3541, .T. ) ;
#4469 = CIRCLE ( 'NONE', #7552, 7.000000000000020428 ) ;
#4470 = AXIS2_PLACEMENT_3D ( 'NONE', #3995, #3428, #6913 ) ;
#4471 = EDGE_CURVE ( 'NONE', #7476, #79, #3512, .T. ) ;
#4472 = CARTESIAN_POINT ( 'NONE',  ( 220.0000000000000000, 9.000000000000001776, 15.00000000000000888 ) ) ;
#4473 = DIRECTION ( 'NONE',  ( 1.000000000000000000, 0.000000000000000000, 0.000000000000000000 ) ) ;
#4474 = ORIENTED_EDGE ( 'NONE', *, *, #833, .T. ) ;
#4475 = CARTESIAN_POINT ( 'NONE',  ( 126.9546976901189623, -19.99999999999997868, 35.00000000000000711 ) ) ;
#4476 = VECTOR ( 'NONE', #1156, 1000.000000000000000 ) ;
#4477 = CARTESIAN_POINT ( 'NONE',  ( -60.70193531918451413, -214.7694783647499719, 94.62885002390540023 ) ) ;
#4478 = MECHANICAL_DESIGN_GEOMETRIC_PRESENTATION_REPRESENTATION (  '', ( #177 ), #1279 ) ;
#4479 = CARTESIAN_POINT ( 'NONE',  ( 40.00000000000000000, -4.163336342344337027E-14, 1.387778780781445676E-14 ) ) ;
#4480 = VECTOR ( 'NONE', #3713, 1000.000000000000000 ) ;
#4481 = LINE ( 'NONE', #1620, #6674 ) ;
#4482 = ORIENTED_EDGE ( 'NONE', *, *, #1352, .F. ) ;
#4483 = ORIENTED_EDGE ( 'NONE', *, *, #4245, .T. ) ;
#4484 = AXIS2_PLACEMENT_3D ( 'NONE', #5354, #2458, #1877 ) ;
#4485 =( GEOMETRIC_REPRESENTATION_CONTEXT ( 3 ) GLOBAL_UNCERTAINTY_ASSIGNED_CONTEXT ( ( #5411 ) ) GLOBAL_UNIT_ASSIGNED_CONTEXT ( ( #1055, #1550, #6247 ) ) REPRESENTATION_CONTEXT ( 'NONE', 'WORKASPACE' ) );
#4486 = AXIS2_PLACEMENT_3D ( 'NONE', #114, #3654, #2912 ) ;
#4487 = DIRECTION ( 'NONE',  ( 1.000000000000000000, -5.551115123125783935E-17, 4.237045877651919561E-33 ) ) ;
#4488 = DIRECTION ( 'NONE',  ( 1.000000000000000000, 0.000000000000000000, 0.000000000000000000 ) ) ;
#4489 = DIRECTION ( 'NONE',  ( 1.751623080406021728E-46, -0.9848077530122080203, 0.1736481776669304977 ) ) ;
#4490 = DIRECTION ( 'NONE',  ( 0.000000000000000000, 0.000000000000000000, 1.000000000000000000 ) ) ;
#4491 = CARTESIAN_POINT ( 'NONE',  ( 3.000000000000002665, 24.90486745229362953, 37.17889356869155648 ) ) ;
#4492 = DIRECTION ( 'NONE',  ( -1.000000000000000000, -0.000000000000000000, -0.000000000000000000 ) ) ;
#4493 = AXIS2_PLACEMENT_3D ( 'NONE', #5311, #615, #2316 ) ;
#4495 = CARTESIAN_POINT ( 'NONE',  ( -61.14025695922334336, -218.0630242524650271, 75.39509193528782305 ) ) ;
#4494 = AXIS2_PLACEMENT_3D ( 'NONE', #3863, #6199, #5364 ) ;
#4496 = ORIENTED_EDGE ( 'NONE', *, *, #3439, .F. ) ;
#4497 = EDGE_LOOP ( 'NONE', ( #3156, #4670 ) ) ;
#4498 = DIRECTION ( 'NONE',  ( 0.000000000000000000, 0.000000000000000000, -1.000000000000000000 ) ) ;
#4499 = AXIS2_PLACEMENT_3D ( 'NONE', #6320, #4519, #3361 ) ;
#4500 = CARTESIAN_POINT ( 'NONE',  ( 188.0000000000000000, -10.95994505756729254, 7.000000000000017764 ) ) ;
#4501 = CARTESIAN_POINT ( 'NONE',  ( -21.49999999999999645, -219.7493155748557285, 95.50692968358183066 ) ) ;
#4502 = ADVANCED_FACE ( 'NONE', ( #498 ), #7600, .T. ) ;
#4503 = CYLINDRICAL_SURFACE ( 'NONE', #414, 12.49999999999999645 ) ;
#4504 = LINE ( 'NONE', #6347, #3102 ) ;
#4505 = EDGE_LOOP ( 'NONE', ( #5044, #32, #5754, #7529 ) ) ;
#4506 = VERTEX_POINT ( 'NONE', #4668 ) ;
#4507 = VECTOR ( 'NONE', #7409, 1000.000000000000000 ) ;
#4508 = EDGE_CURVE ( 'NONE', #2730, #1997, #7537, .T. ) ;
#4509 = CARTESIAN_POINT ( 'NONE',  ( 25.00000000000002132, 73.78679656440357348, 0.9999999999999991118 ) ) ;
#4510 = ORIENTED_EDGE ( 'NONE', *, *, #5900, .T. ) ;
#4511 = CARTESIAN_POINT ( 'NONE',  ( 49.66759159866629858, -24.31912682366575140, 9.999999999997966071 ) ) ;
#4512 = DIRECTION ( 'NONE',  ( 0.000000000000000000, 0.000000000000000000, -1.000000000000000000 ) ) ;
#4513 = ORIENTED_EDGE ( 'NONE', *, *, #6101, .T. ) ;
#4514 =( GEOMETRIC_REPRESENTATION_CONTEXT ( 3 ) GLOBAL_UNCERTAINTY_ASSIGNED_CONTEXT ( ( #3029 ) ) GLOBAL_UNIT_ASSIGNED_CONTEXT ( ( #1374, #4928, #1995 ) ) REPRESENTATION_CONTEXT ( 'NONE', 'WORKASPACE' ) );
#4515 = LINE ( 'NONE', #3934, #3370 ) ;
#4516 = CARTESIAN_POINT ( 'NONE',  ( 188.0000000000000000, -10.62218397927710356, -7.000000000000017764 ) ) ;
#4517 = VERTEX_POINT ( 'NONE', #4708 ) ;
#4518 = VECTOR ( 'NONE', #6705, 1000.000000000000000 ) ;
#4519 = DIRECTION ( 'NONE',  ( -0.9227540886855840618, -2.374784650904215517E-30, 0.3853892730915556841 ) ) ;
#4520 = CARTESIAN_POINT ( 'NONE',  ( 0.000000000000000000, -22.78897920707096247, 12.79060301978498160 ) ) ;
#4521 = ADVANCED_FACE ( 'NONE', ( #5240 ), #5890, .T. ) ;
#4522 = DIRECTION ( 'NONE',  ( 1.853902270198407313E-44, 1.000000000000000000, 0.000000000000000000 ) ) ;
#4523 = EDGE_CURVE ( 'NONE', #429, #496, #2643, .T. ) ;
#4524 = CARTESIAN_POINT ( 'NONE',  ( -32.50000000000002132, -59.26953873475993362, 32.26953873476001888 ) ) ;
#4525 = EDGE_LOOP ( 'NONE', ( #7230, #3360, #5082, #1354 ) ) ;
#4526 = ORIENTED_EDGE ( 'NONE', *, *, #2992, .T. ) ;
#4527 = LINE ( 'NONE', #7019, #1935 ) ;
#4528 = DIRECTION ( 'NONE',  ( 0.000000000000000000, -1.000000000000000000, 0.000000000000000000 ) ) ;
#4529 = CARTESIAN_POINT ( 'NONE',  ( 2.775557561562891351E-14, 86.00000000000000000, 4.999999999999999112 ) ) ;
#4530 = LINE ( 'NONE', #1056, #2030 ) ;
#4531 = CARTESIAN_POINT ( 'NONE',  ( -61.93488458595647472, -223.0627659977873236, 92.05494445931830683 ) ) ;
#4532 = EDGE_CURVE ( 'NONE', #1753, #4443, #2387, .T. ) ;
#4533 = CARTESIAN_POINT ( 'NONE',  ( 2.775557561562891351E-14, 86.00000000000000000, 9.999999999999996447 ) ) ;
#4534 = CARTESIAN_POINT ( 'NONE',  ( 2.775557561562891351E-14, 82.46446609406723383, 6.464466094067257806 ) ) ;
#4535 = CARTESIAN_POINT ( 'NONE',  ( -56.72730684359804343, -218.0630240738404950, 72.54495759198080407 ) ) ;
#4536 = ORIENTED_EDGE ( 'NONE', *, *, #1123, .F. ) ;
#4537 = ORIENTED_EDGE ( 'NONE', *, *, #2439, .F. ) ;
#4538 = CARTESIAN_POINT ( 'NONE',  ( 10.03180245857092423, -218.0630240738404382, 71.94153218116483117 ) ) ;
#4539 = FACE_OUTER_BOUND ( 'NONE', #1576, .T. ) ;
#4540 = CARTESIAN_POINT ( 'NONE',  ( 25.00000000000001421, 80.85786437626907741, 8.071067811865434649 ) ) ;
#4541 = DIRECTION ( 'NONE',  ( 1.000000000000000000, 0.000000000000000000, 0.000000000000000000 ) ) ;
#4542 = DIRECTION ( 'NONE',  ( 1.000000000000000000, 2.465190328815661892E-32, -9.244463733058732095E-33 ) ) ;
#4543 = ORIENTED_EDGE ( 'NONE', *, *, #6352, .T. ) ;
#4544 = EDGE_CURVE ( 'NONE', #1843, #1754, #5856, .T. ) ;
#4545 = ORIENTED_EDGE ( 'NONE', *, *, #656, .T. ) ;
#4546 = CARTESIAN_POINT ( 'NONE',  ( 173.9999999999999716, -10.62218397927710356, -7.000000000000018652 ) ) ;
#4547 = ORIENTED_EDGE ( 'NONE', *, *, #3002, .F. ) ;
#4548 = LINE ( 'NONE', #6886, #4319 ) ;
#4549 = LINE ( 'NONE', #386, #6442 ) ;
#4550 = EDGE_LOOP ( 'NONE', ( #6044, #7318, #1158, #2833 ) ) ;
#4551 = VECTOR ( 'NONE', #4067, 1000.000000000000000 ) ;
#4552 = LINE ( 'NONE', #2928, #6805 ) ;
#4553 = DIRECTION ( 'NONE',  ( 1.000000000000000000, 0.000000000000000000, 5.605193857299269528E-45 ) ) ;
#4554 = ORIENTED_EDGE ( 'NONE', *, *, #2430, .T. ) ;
#4555 = CARTESIAN_POINT ( 'NONE',  ( 21.50000000000000000, 7.347880794884119736E-16, -5.999999999999999112 ) ) ;
#4556 = CLOSED_SHELL ( 'NONE', ( #2052, #6631, #6961, #4865, #7351, #4562, #2774, #4895, #2341, #1728, #3069, #1608, #1573, #1334, #5404, #475, #3085, #7338, #513, #1680, #1732, #4215, #1879, #6503, #2535, #2307, #3813, #1889, #473, #3293 ) ) ;
#4557 = DIRECTION ( 'NONE',  ( 0.000000000000000000, 0.000000000000000000, -1.000000000000000000 ) ) ;
#4558 = DIRECTION ( 'NONE',  ( -1.000000000000000000, -2.624548829666596736E-30, 9.231085635203017994E-31 ) ) ;
#4559 = VERTEX_POINT ( 'NONE', #4632 ) ;
#4560 = EDGE_LOOP ( 'NONE', ( #3593, #3311 ) ) ;
#4561 = VECTOR ( 'NONE', #1739, 1000.000000000000114 ) ;
#4562 = ADVANCED_FACE ( 'NONE', ( #2427 ), #1079, .F. ) ;
#4563 =( BOUNDED_CURVE ( )  B_SPLINE_CURVE ( 3, ( #1600, #6877, #7489, #5731 ),
 .UNSPECIFIED., .F., .T. ) 
 B_SPLINE_CURVE_WITH_KNOTS ( ( 4, 4 ),
 ( 4.712388980384687898, 5.497787143782134400 ),
 .UNSPECIFIED. ) 
 CURVE ( )  GEOMETRIC_REPRESENTATION_ITEM ( )  RATIONAL_B_SPLINE_CURVE ( ( 1.000000000000000000, 0.9492530216741912330, 0.9492530216741912330, 1.000000000000000000 ) ) 
 REPRESENTATION_ITEM ( '' )  );
#4564 = CARTESIAN_POINT ( 'NONE',  ( 49.99999999999998579, 30.03170604878415162, 10.00000000000001243 ) ) ;
#4565 = DIRECTION ( 'NONE',  ( 0.000000000000000000, 0.000000000000000000, -1.000000000000000000 ) ) ;
#4566 = CARTESIAN_POINT ( 'NONE',  ( 2.000000000000001776, -2.465190328815661892E-29, 9.999999999999998224 ) ) ;
#4567 = CARTESIAN_POINT ( 'NONE',  ( -58.56925906381054148, -223.0627927779807749, 94.82172945580802548 ) ) ;
#4568 = CARTESIAN_POINT ( 'NONE',  ( 21.13461073196587137, -223.0630240738404666, 87.73717528194333681 ) ) ;
#4569 = CARTESIAN_POINT ( 'NONE',  ( -64.50000000000000000, -49.37258300203047412, -6.000000000000000888 ) ) ;
#4570 = VECTOR ( 'NONE', #166, 1000.000000000000000 ) ;
#4571 = CARTESIAN_POINT ( 'NONE',  ( -62.25657246635859821, -218.0636273854565275, 76.71444954786895210 ) ) ;
#4572 = ORIENTED_EDGE ( 'NONE', *, *, #6586, .T. ) ;
#4573 = ADVANCED_FACE ( 'NONE', ( #3438 ), #1770, .F. ) ;
#4574 = EDGE_LOOP ( 'NONE', ( #4047, #7087, #2357, #5233 ) ) ;
#4575 = PLANE ( 'NONE',  #906 ) ;
#4576 = CARTESIAN_POINT ( 'NONE',  ( 217.0000000000000000, 56.99999999999999289, 7.000000000000022204 ) ) ;
#4577 = CARTESIAN_POINT ( 'NONE',  ( -16.49999999999996447, 0.000000000000000000, 6.000000000000000888 ) ) ;
#4578 = FACE_OUTER_BOUND ( 'NONE', #1838, .T. ) ;
#4579 = FACE_OUTER_BOUND ( 'NONE', #3701, .T. ) ;
#4580 = VECTOR ( 'NONE', #2231, 1000.000000000000000 ) ;
#4581 = ORIENTED_EDGE ( 'NONE', *, *, #5177, .F. ) ;
#4582 = ORIENTED_EDGE ( 'NONE', *, *, #5414, .F. ) ;
#4583 = LINE ( 'NONE', #1429, #4518 ) ;
#4584 = DIRECTION ( 'NONE',  ( -1.000000000000000000, -2.624548829666596736E-30, 9.231085635203017994E-31 ) ) ;
#4585 = ORIENTED_EDGE ( 'NONE', *, *, #5038, .T. ) ;
#4586 = EDGE_CURVE ( 'NONE', #6424, #1631, #6394, .T. ) ;
#4587 = DIRECTION ( 'NONE',  ( 1.000000000000000000, 0.000000000000000000, 7.663350976776343357E-46 ) ) ;
#4588 = CARTESIAN_POINT ( 'NONE',  ( 10.03180245857092423, -218.0630240738404382, 71.94153218116483117 ) ) ;
#4589 = ORIENTED_EDGE ( 'NONE', *, *, #5509, .T. ) ;
#4590 = VERTEX_POINT ( 'NONE', #6971 ) ;
#4591 = CARTESIAN_POINT ( 'NONE',  ( 25.00000000000000711, 40.21320343559642652, 10.99999999999999467 ) ) ;
#4592 = CARTESIAN_POINT ( 'NONE',  ( 27.14230383934499002, -218.4648600334251682, 89.55655311265203977 ) ) ;
#4593 = ORIENTED_EDGE ( 'NONE', *, *, #4102, .T. ) ;
#4594 = EDGE_CURVE ( 'NONE', #1397, #2880, #1695, .T. ) ;
#4595 = CARTESIAN_POINT ( 'NONE',  ( -53.06880420804609599, -218.8824061789517259, 72.16108495452192528 ) ) ;
#4596 = CARTESIAN_POINT ( 'NONE',  ( -28.15685424949236548, -218.0630240738404666, 95.20959099461347819 ) ) ;
#4597 = CARTESIAN_POINT ( 'NONE',  ( 0.000000000000000000, 0.000000000000000000, 35.00000000000000000 ) ) ;
#4598 = CIRCLE ( 'NONE', #6683, 23.99999999999999289 ) ;
#4599 = ORIENTED_EDGE ( 'NONE', *, *, #7454, .F. ) ;
#4600 = CARTESIAN_POINT ( 'NONE',  ( 3.000000000000002665, 30.03170604878415162, 13.00000000000001066 ) ) ;
#4601 = CIRCLE ( 'NONE', #3740, 4.999999999999999112 ) ;
#4602 = VECTOR ( 'NONE', #5646, 1000.000000000000000 ) ;
#4603 = CARTESIAN_POINT ( 'NONE',  ( -32.50000000000002842, -49.37258300203047412, 0.000000000000000000 ) ) ;
#4604 = ADVANCED_FACE ( 'NONE', ( #6550 ), #4349, .T. ) ;
#4605 = CARTESIAN_POINT ( 'NONE',  ( -63.06750362476648775, -223.0623716789916102, 90.42757439449754031 ) ) ;
#4606 = DIRECTION ( 'NONE',  ( 0.000000000000000000, 0.000000000000000000, 1.000000000000000000 ) ) ;
#4607 = LINE ( 'NONE', #3457, #612 ) ;
#4608 = EDGE_CURVE ( 'NONE', #3994, #208, #7268, .T. ) ;
#4609 = CARTESIAN_POINT ( 'NONE',  ( -63.61353958389151586, -218.0630304217399669, 79.17370859764169211 ) ) ;
#4610 = VECTOR ( 'NONE', #7497, 1000.000000000000000 ) ;
#4611 = CIRCLE ( 'NONE', #2517, 6.000000000000003553 ) ;
#4612 = TOROIDAL_SURFACE ( 'NONE', #7548, 6.000000000000000000, 3.000000000000000000 ) ;
#4613 =( BOUNDED_CURVE ( )  B_SPLINE_CURVE ( 3, ( #2844, #5194, #7531, #572 ),
 .UNSPECIFIED., .F., .T. ) 
 B_SPLINE_CURVE_WITH_KNOTS ( ( 4, 4 ),
 ( 4.712388980384690562, 6.283185307179586232 ),
 .UNSPECIFIED. ) 
 CURVE ( )  GEOMETRIC_REPRESENTATION_ITEM ( )  RATIONAL_B_SPLINE_CURVE ( ( 1.000000000000000000, 0.8047378541243652705, 0.8047378541243652705, 1.000000000000000000 ) ) 
 REPRESENTATION_ITEM ( '' )  );
#4614 = VERTEX_POINT ( 'NONE', #1957 ) ;
#4615 = CARTESIAN_POINT ( 'NONE',  ( 3.000000000000002665, -60.00000000000000000, 0.000000000000000000 ) ) ;
#4616 = FACE_OUTER_BOUND ( 'NONE', #4010, .T. ) ;
#4617 = CIRCLE ( 'NONE', #1290, 3.000000000000000444 ) ;
#4618 = FACE_OUTER_BOUND ( 'NONE', #5726, .T. ) ;
#4619 = CARTESIAN_POINT ( 'NONE',  ( 217.0000000000000000, -15.08392021690037943, 12.00000000000000711 ) ) ;
#4620 = VECTOR ( 'NONE', #3004, 1000.000000000000000 ) ;
#4621 = AXIS2_PLACEMENT_3D ( 'NONE', #2638, #3838, #6135 ) ;
#4622 = CARTESIAN_POINT ( 'NONE',  ( 186.0399638286351376, -8.214460233858028815, 13.50000000000791012 ) ) ;
#4623 = EDGE_CURVE ( 'NONE', #6273, #5270, #2626, .T. ) ;
#4624 = EDGE_CURVE ( 'NONE', #1413, #7513, #4705, .T. ) ;
#4625 = ORIENTED_EDGE ( 'NONE', *, *, #2353, .T. ) ;
#4626 = AXIS2_PLACEMENT_3D ( 'NONE', #6820, #6239, #1577 ) ;
#4627 = EDGE_LOOP ( 'NONE', ( #5625, #6055, #5336, #6699 ) ) ;
#4628 = DIRECTION ( 'NONE',  ( 0.000000000000000000, 0.000000000000000000, 1.000000000000000000 ) ) ;
#4629 = DIRECTION ( 'NONE',  ( -1.681558157189779738E-44, 0.000000000000000000, -1.000000000000000000 ) ) ;
#4630 = VERTEX_POINT ( 'NONE', #3917 ) ;
#4631 = CARTESIAN_POINT ( 'NONE',  ( 217.0000000000000000, 56.99999999999999289, 7.000000000000022204 ) ) ;
#4632 = CARTESIAN_POINT ( 'NONE',  ( 217.0000000000000000, 18.04196010845019060, 12.50000000000000711 ) ) ;
#4633 = EDGE_LOOP ( 'NONE', ( #1989, #3600, #6619, #6468 ) ) ;
#4634 = VERTEX_POINT ( 'NONE', #5112 ) ;
#4635 = CIRCLE ( 'NONE', #1182, 6.000000000000000888 ) ;
#4636 = CARTESIAN_POINT ( 'NONE',  ( 217.0000000000000000, 56.99999999999999289, 10.00000000000002132 ) ) ;
#4637 = CARTESIAN_POINT ( 'NONE',  ( 17.67236366837565953, -212.7665347604138617, 94.27567702561840690 ) ) ;
#4638 = ORIENTED_EDGE ( 'NONE', *, *, #3630, .T. ) ;
#4639 = APPLICATION_PROTOCOL_DEFINITION ( 'draft international standard', 'automotive_design', 1998, #7027 ) ;
#4640 = CARTESIAN_POINT ( 'NONE',  ( 217.0000000000000000, -2.312964634635744633E-15, 7.000000000000002665 ) ) ;
#4641 = LINE ( 'NONE', #6979, #1504 ) ;
#4642 = AXIS2_PLACEMENT_3D ( 'NONE', #2559, #2060, #2129 ) ;
#4643 = VERTEX_POINT ( 'NONE', #6252 ) ;
#4644 = ORIENTED_EDGE ( 'NONE', *, *, #7222, .T. ) ;
#4645 = EDGE_CURVE ( 'NONE', #2786, #2919, #5681, .T. ) ;
#4646 = CIRCLE ( 'NONE', #5012, 5.999999999999999112 ) ;
#4647 = DIRECTION ( 'NONE',  ( 0.000000000000000000, -1.000000000000000000, -1.221245327087672392E-15 ) ) ;
#4648 = DIRECTION ( 'NONE',  ( 0.7071067811865461294, 1.855836275012464020E-30, -0.7071067811865489050 ) ) ;
#4649 = LINE ( 'NONE', #4723, #6579 ) ;
#4650 = CARTESIAN_POINT ( 'NONE',  ( 21.50149794217480093, -218.0630240738406087, 83.70532250279403286 ) ) ;
#4651 = LINE ( 'NONE', #1710, #4551 ) ;
#4652 = CARTESIAN_POINT ( 'NONE',  ( -15.92209785380265608, -113.7796841263388501, 41.77968412633906325 ) ) ;
#4653 = EDGE_CURVE ( 'NONE', #3524, #2601, #5725, .T. ) ;
#4654 = ORIENTED_EDGE ( 'NONE', *, *, #7048, .F. ) ;
#4655 = CARTESIAN_POINT ( 'NONE',  ( -10.49999999999996625, -60.68629150101523351, -11.31370849898472031 ) ) ;
#4656 = CARTESIAN_POINT ( 'NONE',  ( -16.49999999999996447, -49.37258300203045280, -2.775557561562891351E-14 ) ) ;
#4657 = CARTESIAN_POINT ( 'NONE',  ( -18.18629150101523706, -223.0630240738405234, 96.09122589815579829 ) ) ;
#4658 = CARTESIAN_POINT ( 'NONE',  ( 10.39932558417664410, -221.3963574071637197, 95.79734759697325330 ) ) ;
#4659 = DIRECTION ( 'NONE',  ( -0.4999999999999976130, -0.000000000000000000, -0.8660254037844399289 ) ) ;
#4660 = VERTEX_POINT ( 'NONE', #6236 ) ;
#4661 = PRODUCT_DEFINITION_SHAPE ( 'NONE', 'NONE',  #7605 ) ;
#4662 = EDGE_LOOP ( 'NONE', ( #6735, #5541, #356, #1727 ) ) ;
#4663 = EDGE_CURVE ( 'NONE', #1397, #5394, #1640, .T. ) ;
#4664 = FACE_BOUND ( 'NONE', #2142, .T. ) ;
#4665 = CARTESIAN_POINT ( 'NONE',  ( 188.0000000000000000, -10.62218397927710356, -7.000000000000017764 ) ) ;
#4666 = VERTEX_POINT ( 'NONE', #7352 ) ;
#4667 = CARTESIAN_POINT ( 'NONE',  ( 50.01367358680484188, -23.17418217178283868, 9.999999999989126920 ) ) ;
#4668 = CARTESIAN_POINT ( 'NONE',  ( -16.49999999999996447, 6.938893903907228378E-15, -16.00000000000001421 ) ) ;
#4669 = ORIENTED_EDGE ( 'NONE', *, *, #1814, .F. ) ;
#4670 = ORIENTED_EDGE ( 'NONE', *, *, #5457, .T. ) ;
#4671 = ADVANCED_FACE ( 'NONE', ( #716 ), #5554, .T. ) ;
#4672 = CARTESIAN_POINT ( 'NONE',  ( 21.50000000000000000, -60.68629150101523351, -11.31370849898472031 ) ) ;
#4673 = CARTESIAN_POINT ( 'NONE',  ( 27.04900473833201957, -222.6575489669630770, 90.39048551345003091 ) ) ;
#4674 = ORIENTED_EDGE ( 'NONE', *, *, #5413, .F. ) ;
#4675 = EDGE_CURVE ( 'NONE', #1932, #6366, #2783, .T. ) ;
#4676 = APPLICATION_PROTOCOL_DEFINITION ( 'draft international standard', 'automotive_design', 1998, #3096 ) ;
#4677 = DIRECTION ( 'NONE',  ( -0.000000000000000000, -0.000000000000000000, 1.000000000000000000 ) ) ;
#4678 = CYLINDRICAL_SURFACE ( 'NONE', #901, 2.999999999999999112 ) ;
#4679 = CIRCLE ( 'NONE', #128, 10.00000000000000355 ) ;
#4680 = ORIENTED_EDGE ( 'NONE', *, *, #2073, .F. ) ;
#4681 = CARTESIAN_POINT ( 'NONE',  ( 25.00000000000000000, 31.53553390593274841, 6.464466094067257806 ) ) ;
#4682 = CARTESIAN_POINT ( 'NONE',  ( 1.387778780781445676E-14, 33.14213562373091548, 8.071067811865429320 ) ) ;
#4683 = AXIS2_PLACEMENT_3D ( 'NONE', #3576, #645, #5343 ) ;
#4684 = CARTESIAN_POINT ( 'NONE',  ( 50.51471862576143224, 30.03170604878414807, 10.00000000000001066 ) ) ;
#4685 = DIRECTION ( 'NONE',  ( -1.000000000000000000, 5.551115123125783935E-17, -4.237045877651919561E-33 ) ) ;
#4686 = CARTESIAN_POINT ( 'NONE',  ( 17.02959548118919031, -223.0630240738405234, 93.94559367446881026 ) ) ;
#4687 = CARTESIAN_POINT ( 'NONE',  ( -21.50000000000000000, -69.31370849898461017, 42.31370849898474518 ) ) ;
#4688 = EDGE_CURVE ( 'NONE', #3412, #6889, #2048, .T. ) ;
#4689 = EDGE_CURVE ( 'NONE', #7339, #3503, #3070, .T. ) ;
#4690 = VECTOR ( 'NONE', #285, 1000.000000000000114 ) ;
#4691 = ORIENTED_EDGE ( 'NONE', *, *, #2448, .F. ) ;
#4692 = ORIENTED_EDGE ( 'NONE', *, *, #5314, .F. ) ;
#4693 =( NAMED_UNIT ( * ) PLANE_ANGLE_UNIT ( ) SI_UNIT ( $, .RADIAN. ) );
#4694 = CARTESIAN_POINT ( 'NONE',  ( 3.000000000000000000, -56.99999999999999289, 3.000000000000000444 ) ) ;
#4695 = CARTESIAN_POINT ( 'NONE',  ( 36.00000000000000000, 0.000000000000000000, 1.387778780781445676E-14 ) ) ;
#4696 = DIRECTION ( 'NONE',  ( -1.000000000000000000, -0.000000000000000000, -0.000000000000000000 ) ) ;
#4697 = DIRECTION ( 'NONE',  ( 0.000000000000000000, 0.000000000000000000, 1.000000000000000000 ) ) ;
#4698 = ADVANCED_FACE ( 'NONE', ( #3318 ), #5664, .T. ) ;
#4699 = ORIENTED_EDGE ( 'NONE', *, *, #6155, .F. ) ;
#4700 = ORIENTED_EDGE ( 'NONE', *, *, #3053, .T. ) ;
#4701 = DIRECTION ( 'NONE',  ( 0.000000000000000000, -0.000000000000000000, 1.000000000000000000 ) ) ;
#4702 = AXIS2_PLACEMENT_3D ( 'NONE', #5492, #6534, #7142 ) ;
#4703 = DIRECTION ( 'NONE',  ( -1.000000000000000000, -2.624548829666596736E-30, 9.231085635203017994E-31 ) ) ;
#4704 = ORIENTED_EDGE ( 'NONE', *, *, #4645, .F. ) ;
#4705 = B_SPLINE_CURVE_WITH_KNOTS ( 'NONE', 3,
 ( #4893, #232, #4239, #695, #1267, #5430, #1419, #5393, #947, #5967, #123, #160, #3116, #5470, #3299, #6004, #2462, #368, #2542, #200, #3083, #1375, #4818, #4311, #6652, #4929, #3881, #2573, #4204, #2713, #3736, #6617, #7156, #7120, #6584, #1996, #1847, #1308, #3667, #4856, #6078, #7195, #805, #1925, #4277, #1339, #3155, #5506, #3700, #1591, #2260, #1096, #5145, #7520, #7403, #3458, #2793, #6871, #5799, #3991, #4609, #450, #520, #7484, #2750, #2868, #5762, #2221, #4571, #4034, #1060, #7448, #6909, #5220, #2831, #2181, #6341, #4495, #981, #3953, #5184, #1630, #6953, #7560, #3423, #6379, #2138, #1020, #481, #3339, #5065, #4535, #6834, #1677, #6294, #1556 ),
 .UNSPECIFIED., .F., .F.,
 ( 4, 2, 2, 2, 1, 1, 2, 2, 2, 2, 2, 1, 1, 1, 2, 2, 2, 2, 2, 1, 1, 1, 1, 1, 2, 2, 2, 2, 2, 2, 2, 2, 2, 2, 1, 1, 1, 1, 1, 2, 2, 2, 2, 2, 1, 1, 1, 2, 2, 2, 2, 2, 1, 1, 2, 2, 2, 4 ),
 ( 0.000000000000000000, 0.06250000000003484713, 0.09375000000005226375, 0.1093750000000608125, 0.1171875000000650868, 0.1210937500000670158, 0.1230468750000682093, 0.1250000000000693889, 0.1875000000000952849, 0.2187500000001082467, 0.2343750000001147138, 0.2421875000001181555, 0.2460937500001195155, 0.2480468750001201816, 0.2490234375001202927, 0.2500000000001204037, 0.3125000000001556533, 0.3437500000001734168, 0.3593750000001822986, 0.3671875000001867395, 0.3710937500001889600, 0.3730468750001900702, 0.3740234375001909028, 0.3745117187501913469, 0.3747558593751918465, 0.3750000000001923461, 0.4375000000002062239, 0.4687500000002127187, 0.4843750000002159384, 0.4921875000002171041, 0.5000000000002181588, 0.5625000000002263745, 0.5937500000002299272, 0.6093750000002309264, 0.6171875000002320366, 0.6210937500002324807, 0.6230468750002324807, 0.6240234375002313705, 0.6245117187502307043, 0.6247558593752309264, 0.6250000000002310374, 0.6875000000002089440, 0.7187500000001981748, 0.7343750000001931788, 0.7421875000001901812, 0.7460937500001887379, 0.7480468750001882938, 0.7490234375001878497, 0.7500000000001872946, 0.8125000000001266764, 0.8437500000000963674, 0.8593750000000810463, 0.8671875000000730527, 0.8710937500000696110, 0.8730468750000682787, 0.8750000000000670575, 0.9375000000000335287, 1.000000000000000000 ),
 .UNSPECIFIED. ) ;
#4706 = ADVANCED_FACE ( 'NONE', ( #5049 ), #929, .F. ) ;
#4707 = CARTESIAN_POINT ( 'NONE',  ( 47.40604585759381706, -25.88825784476160052, 9.999999999998642863 ) ) ;
#4708 = CARTESIAN_POINT ( 'NONE',  ( -29.35769912250765046, -65.63670350735181103, 38.63670350735190340 ) ) ;
#4709 = EDGE_CURVE ( 'NONE', #628, #2172, #957, .T. ) ;
#4710 = VERTEX_POINT ( 'NONE', #5417 ) ;
#4711 = VECTOR ( 'NONE', #1500, 1000.000000000000114 ) ;
#4712 = ORIENTED_EDGE ( 'NONE', *, *, #4384, .F. ) ;
#4713 = CARTESIAN_POINT ( 'NONE',  ( -10.49999999999996803, 7.347880794884121708E-16, -6.000000000000000888 ) ) ;
#4714 = CARTESIAN_POINT ( 'NONE',  ( 26.99135978879997566, -227.6251019015761301, 80.18334626974973389 ) ) ;
#4715 = EDGE_LOOP ( 'NONE', ( #605, #1697, #2102, #3280 ) ) ;
#4716 = CARTESIAN_POINT ( 'NONE',  ( 220.0000000000000000, -9.000000000000001776, 12.00000000000000888 ) ) ;
#4717 = PLANE ( 'NONE',  #2000 ) ;
#4718 = ADVANCED_FACE ( 'NONE', ( #2485 ), #5683, .F. ) ;
#4719 = ORIENTED_EDGE ( 'NONE', *, *, #2213, .F. ) ;
#4720 = AXIS2_PLACEMENT_3D ( 'NONE', #508, #6441, #664 ) ;
#4721 = FACE_OUTER_BOUND ( 'NONE', #569, .T. ) ;
#4722 = FACE_OUTER_BOUND ( 'NONE', #3436, .T. ) ;
#4723 = CARTESIAN_POINT ( 'NONE',  ( 25.00000000000000711, 40.21320343559642652, 5.999999999999996447 ) ) ;
#4724 = CARTESIAN_POINT ( 'NONE',  ( 217.0000000000000000, 56.99999999999999289, 7.000000000000021316 ) ) ;
#4725 = CARTESIAN_POINT ( 'NONE',  ( 14.95763687199172054, -223.0630240738405519, 95.12286150347453884 ) ) ;
#4726 = LINE ( 'NONE', #4147, #7364 ) ;
#4727 = AXIS2_PLACEMENT_3D ( 'NONE', #6008, #5316, #4246 ) ;
#4728 = AXIS2_PLACEMENT_3D ( 'NONE', #1718, #2950, #683 ) ;
#4729 = VERTEX_POINT ( 'NONE', #5202 ) ;
#4730 = DIRECTION ( 'NONE',  ( 0.000000000000000000, 0.000000000000000000, 1.000000000000000000 ) ) ;
#4731 = FACE_OUTER_BOUND ( 'NONE', #949, .T. ) ;
#4732 = DIRECTION ( 'NONE',  ( -0.4999999999999967804, 2.003086131649549845E-15, -0.8660254037844405950 ) ) ;
#4733 = DIRECTION ( 'NONE',  ( -0.000000000000000000, 1.000000000000000000, -0.000000000000000000 ) ) ;
#4734 = CARTESIAN_POINT ( 'NONE',  ( 189.3320144560679239, -7.156359838973473941, 15.60099947390724928 ) ) ;
#4735 = AXIS2_PLACEMENT_3D ( 'NONE', #4924, #195, #5007 ) ;
#4736 = AXIS2_PLACEMENT_3D ( 'NONE', #5115, #2186, #1024 ) ;
#4737 = AXIS2_PLACEMENT_3D ( 'NONE', #1819, #1700, #5933 ) ;
#4738 = VERTEX_POINT ( 'NONE', #4636 ) ;
#4739 = ORIENTED_EDGE ( 'NONE', *, *, #7327, .F. ) ;
#4740 = AXIS2_PLACEMENT_3D ( 'NONE', #526, #6346, #5228 ) ;
#4741 = ADVANCED_BREP_SHAPE_REPRESENTATION ( '', ( #6351, #1914 ), #1662 ) ;
#4742 = EDGE_CURVE ( 'NONE', #6255, #1259, #2164, .T. ) ;
#4743 = AXIS2_PLACEMENT_3D ( 'NONE', #5254, #3484, #670 ) ;
#4744 = VECTOR ( 'NONE', #1801, 1000.000000000000114 ) ;
#4745 = DIRECTION ( 'NONE',  ( 0.000000000000000000, 0.000000000000000000, 1.000000000000000000 ) ) ;
#4746 = FACE_OUTER_BOUND ( 'NONE', #4715, .T. ) ;
#4747 = VERTEX_POINT ( 'NONE', #6436 ) ;
#4748 = CARTESIAN_POINT ( 'NONE',  ( -70.04900473833201602, -225.0595978535631616, 79.55554317441176693 ) ) ;
#4749 = DIRECTION ( 'NONE',  ( 0.000000000000000000, -1.000000000000000000, 0.000000000000000000 ) ) ;
#4750 = DIRECTION ( 'NONE',  ( -1.000000000000000000, -0.000000000000000000, -0.000000000000000000 ) ) ;
#4751 = AXIS2_PLACEMENT_3D ( 'NONE', #3092, #7236, #277 ) ;
#4752 = ORIENTED_EDGE ( 'NONE', *, *, #2807, .F. ) ;
#4753 = ORIENTED_EDGE ( 'NONE', *, *, #4532, .T. ) ;
#4754 = ADVANCED_FACE ( 'NONE', ( #3404 ), #7582, .T. ) ;
#4755 = CARTESIAN_POINT ( 'NONE',  ( 47.00000000000000000, -25.78715168812825098, 12.89530150989249435 ) ) ;
#4756 = CARTESIAN_POINT ( 'NONE',  ( 10.10580595754474764, -214.7694783647500287, 94.62885002390419231 ) ) ;
#4757 = PRODUCT_CONTEXT ( 'NONE', #4036, 'mechanical' ) ;
#4758 = DIRECTION ( 'NONE',  ( -0.000000000000000000, -0.000000000000000000, 1.000000000000000000 ) ) ;
#4759 = CYLINDRICAL_SURFACE ( 'NONE', #45, 4.999999999999999112 ) ;
#4760 = ORIENTED_EDGE ( 'NONE', *, *, #6156, .F. ) ;
#4761 = AXIS2_PLACEMENT_3D ( 'NONE', #6257, #1561, #5035 ) ;
#4762 = CARTESIAN_POINT ( 'NONE',  ( 3.000000000000002665, 60.00000000000000000, 2.204364238465235507E-14 ) ) ;
#4763 = EDGE_CURVE ( 'NONE', #4080, #3340, #582, .T. ) ;
#4764 = CARTESIAN_POINT ( 'NONE',  ( 220.0000000000000000, -3.000000000000000888, 35.00000000000000000 ) ) ;
#4765 = AXIS2_PLACEMENT_3D ( 'NONE', #6077, #7229, #6651 ) ;
#4766 = CARTESIAN_POINT ( 'NONE',  ( 12.50000000000000355, 101.5000000000000000, -1.214306433183764966E-14 ) ) ;
#4767 = CARTESIAN_POINT ( 'NONE',  ( 36.00000000000000000, 0.000000000000000000, 6.000000000000015099 ) ) ;
#4768 = CARTESIAN_POINT ( 'NONE',  ( 188.6380400399839061, 7.242640687119284770, 15.00000000000001066 ) ) ;
#4769 = VECTOR ( 'NONE', #3467, 1000.000000000000000 ) ;
#4770 = ORIENTED_EDGE ( 'NONE', *, *, #6184, .F. ) ;
#4771 = CARTESIAN_POINT ( 'NONE',  ( 0.000000000000000000, 0.000000000000000000, -9.999999999999994671 ) ) ;
#4772 = EDGE_CURVE ( 'NONE', #5471, #5437, #3517, .T. ) ;
#4773 = SURFACE_SIDE_STYLE ('',( #25 ) ) ;
#4774 = CARTESIAN_POINT ( 'NONE',  ( -10.49999999999998579, -61.67366827531365203, 34.67366827531376572 ) ) ;
#4775 = DIRECTION ( 'NONE',  ( 5.551115123125782702E-17, 1.000000000000000000, 0.000000000000000000 ) ) ;
#4776 = DIRECTION ( 'NONE',  ( 1.000000000000000000, 0.000000000000000000, 0.000000000000000000 ) ) ;
#4777 = AXIS2_PLACEMENT_3D ( 'NONE', #7036, #2920, #4745 ) ;
#4778 = ORIENTED_EDGE ( 'NONE', *, *, #20, .T. ) ;
#4779 = ORIENTED_EDGE ( 'NONE', *, *, #207, .F. ) ;
#4780 = CARTESIAN_POINT ( 'NONE',  ( 193.5000000000000000, -39.99999999999999289, 0.000000000000000000 ) ) ;
#4781 = CARTESIAN_POINT ( 'NONE',  ( 3.000000000000002665, -56.99999999999999289, 3.000000000000000444 ) ) ;
#4782 = ORIENTED_EDGE ( 'NONE', *, *, #7568, .F. ) ;
#4783 = CARTESIAN_POINT ( 'NONE',  ( -53.29386626619290723, -223.8662738488881985, 73.49650827186496826 ) ) ;
#4784 = SURFACE_SIDE_STYLE ('',( #38 ) ) ;
#4785 = CARTESIAN_POINT ( 'NONE',  ( -21.50000000000000000, -223.0630240738404950, 96.09122589815579829 ) ) ;
#4786 = EDGE_CURVE ( 'NONE', #2388, #5318, #6682, .T. ) ;
#4787 = EDGE_LOOP ( 'NONE', ( #3239, #938 ) ) ;
#4788 = EDGE_LOOP ( 'NONE', ( #5670, #1121 ) ) ;
#4789 = CARTESIAN_POINT ( 'NONE',  ( 0.000000000000000000, 0.000000000000000000, -9.999999999999994671 ) ) ;
#4790 = CARTESIAN_POINT ( 'NONE',  ( 17.68960140267981984, -218.8824061789507880, 72.16108495452550642 ) ) ;
#4791 = ORIENTED_EDGE ( 'NONE', *, *, #4932, .T. ) ;
#4792 = PRODUCT_CONTEXT ( 'NONE', #6922, 'mechanical' ) ;
#4793 = CARTESIAN_POINT ( 'NONE',  ( 185.0000000000000000, -39.99999999999999289, 0.000000000000000000 ) ) ;
#4794 = CARTESIAN_POINT ( 'NONE',  ( 220.0000000000000000, -15.00000000000000355, 12.00000000000000711 ) ) ;
#4795 = VERTEX_POINT ( 'NONE', #5860 ) ;
#4796 = DIRECTION ( 'NONE',  ( 1.000000000000000000, 0.000000000000000000, 0.000000000000000000 ) ) ;
#4797 = DIRECTION ( 'NONE',  ( 0.7071067811865435759, -8.465450562766819607E-16, 0.7071067811865514585 ) ) ;
#4798 = CARTESIAN_POINT ( 'NONE',  ( 200.0000000000000000, 0.000000000000000000, 0.000000000000000000 ) ) ;
#4799 = FACE_OUTER_BOUND ( 'NONE', #4400, .T. ) ;
#4800 = DIRECTION ( 'NONE',  ( 0.000000000000000000, 0.000000000000000000, -1.000000000000000000 ) ) ;
#4801 = ADVANCED_FACE ( 'NONE', ( #2201 ), #2778, .T. ) ;
#4802 = VECTOR ( 'NONE', #2907, 1000.000000000000000 ) ;
#4803 = PLANE ( 'NONE',  #2658 ) ;
#4804 = DIRECTION ( 'NONE',  ( 2.465190328815661892E-32, 1.000000000000000000, 1.193489751472043281E-15 ) ) ;
#4805 = FACE_OUTER_BOUND ( 'NONE', #2467, .T. ) ;
#4806 = CARTESIAN_POINT ( 'NONE',  ( 187.5208830142895238, 7.524469495810456543, 15.00000000000001243 ) ) ;
#4807 = CARTESIAN_POINT ( 'NONE',  ( -64.50000000000000000, -113.7796841263389211, 41.77968412633906325 ) ) ;
#4808 = VECTOR ( 'NONE', #6018, 1000.000000000000114 ) ;
#4809 = AXIS2_PLACEMENT_3D ( 'NONE', #4976, #7316, #3058 ) ;
#4810 = EDGE_CURVE ( 'NONE', #7468, #597, #4552, .T. ) ;
#4811 = EDGE_LOOP ( 'NONE', ( #1890, #3327, #3328 ) ) ;
#4812 = ORIENTED_EDGE ( 'NONE', *, *, #4951, .T. ) ;
#4813 = VECTOR ( 'NONE', #209, 1000.000000000000000 ) ;
#4814 = CARTESIAN_POINT ( 'NONE',  ( -53.03180245857092956, -218.0630240738404950, 71.94153218116483117 ) ) ;
#4815 = CARTESIAN_POINT ( 'NONE',  ( -53.29386626619290723, -219.0153713307822443, 95.37751551101598579 ) ) ;
#4816 = CARTESIAN_POINT ( 'NONE',  ( -70.25616595088855831, -213.3481074634626964, 88.53882300612518463 ) ) ;
#4817 = LINE ( 'NONE', #652, #2842 ) ;
#4818 = CARTESIAN_POINT ( 'NONE',  ( -61.25564343853275773, -218.0630214440888608, 91.79691897930752020 ) ) ;
#4819 = AXIS2_PLACEMENT_3D ( 'NONE', #6508, #1924, #6616 ) ;
#4820 = ORIENTED_EDGE ( 'NONE', *, *, #6731, .T. ) ;
#4821 = ORIENTED_EDGE ( 'NONE', *, *, #4688, .T. ) ;
#4822 = APPLICATION_CONTEXT ( 'automotive_design' ) ;
#4823 = VECTOR ( 'NONE', #4990, 1000.000000000000000 ) ;
#4824 = DIRECTION ( 'NONE',  ( 0.000000000000000000, 0.000000000000000000, -1.000000000000000000 ) ) ;
#4825 = CARTESIAN_POINT ( 'NONE',  ( 10.43756829269602804, -227.0484711946324126, 74.34917548081359939 ) ) ;
#4826 = ORIENTED_EDGE ( 'NONE', *, *, #4151, .F. ) ;
#4827 = CARTESIAN_POINT ( 'NONE',  ( 217.0000000000000000, 15.08392021690038121, 15.00000000000000888 ) ) ;
#4828 = PLANE ( 'NONE',  #75 ) ;
#4829 = CIRCLE ( 'NONE', #639, 15.99999999999999645 ) ;
#4830 = ORIENTED_EDGE ( 'NONE', *, *, #1141, .F. ) ;
#4831 = DIRECTION ( 'NONE',  ( 0.000000000000000000, 0.03489949670250346025, 0.9993908270190956511 ) ) ;
#4832 = EDGE_CURVE ( 'NONE', #2722, #5727, #5701, .T. ) ;
#4833 = DIRECTION ( 'NONE',  ( -0.6444004775717536715, 0.5407162030609466985, -0.5407162030609483638 ) ) ;
#4834 = VERTEX_POINT ( 'NONE', #5703 ) ;
#4835 = CARTESIAN_POINT ( 'NONE',  ( 26.99999999999999289, 0.000000000000000000, -3.000000000000002665 ) ) ;
#4836 = CARTESIAN_POINT ( 'NONE',  ( 3.000000000000002665, 56.99999999999999289, 2.204364238465235507E-14 ) ) ;
#4837 = ORIENTED_EDGE ( 'NONE', *, *, #5243, .F. ) ;
#4838 = AXIS2_PLACEMENT_3D ( 'NONE', #2857, #6557, #5866 ) ;
#4839 = DIRECTION ( 'NONE',  ( -5.605193857299269528E-45, 0.000000000000000000, 1.000000000000000000 ) ) ;
#4840 = ADVANCED_FACE ( 'NONE', ( #5165 ), #7505, .F. ) ;
#4841 = DIRECTION ( 'NONE',  ( 1.000000000000000000, 2.624548829666596736E-30, -9.231085635203017994E-31 ) ) ;
#4842 = CARTESIAN_POINT ( 'NONE',  ( 0.000000000000000000, 78.92893218813448186, 2.928932188134520498 ) ) ;
#4843 = LINE ( 'NONE', #5913, #68 ) ;
#4844 = CARTESIAN_POINT ( 'NONE',  ( -62.71099586730315423, -223.0636365687223872, 78.56832023356531636 ) ) ;
#4845 = CARTESIAN_POINT ( 'NONE',  ( 186.7339382447161711, -5.312719677946581065, 14.70199894781319649 ) ) ;
#4846 = CIRCLE ( 'NONE', #3241, 3.000000000000000000 ) ;
#4847 = EDGE_LOOP ( 'NONE', ( #838, #1481, #4394, #6926, #165 ) ) ;
#4848 = EDGE_LOOP ( 'NONE', ( #5819, #5347 ) ) ;
#4849 = DIRECTION ( 'NONE',  ( 0.000000000000000000, -1.000000000000000000, -1.221245327087672392E-15 ) ) ;
#4850 = DIRECTION ( 'NONE',  ( 0.000000000000000000, 0.000000000000000000, -1.000000000000000000 ) ) ;
#4851 = AXIS2_PLACEMENT_3D ( 'NONE', #5379, #2335, #7141 ) ;
#4852 = EDGE_CURVE ( 'NONE', #6942, #2264, #4515, .T. ) ;
#4853 = EDGE_CURVE ( 'NONE', #2663, #3579, #5128, .T. ) ;
#4854 = DIRECTION ( 'NONE',  ( 1.000000000000000000, -1.804112415015879773E-15, 4.237045877651875086E-33 ) ) ;
#4855 = CARTESIAN_POINT ( 'NONE',  ( 170.0000000000000000, -11.00000000000000355, 8.660254037844387298 ) ) ;
#4856 = CARTESIAN_POINT ( 'NONE',  ( -63.70683303208141268, -218.0630240594568647, 87.95135174290737723 ) ) ;
#4857 = ORIENTED_EDGE ( 'NONE', *, *, #3053, .F. ) ;
#4858 = AXIS2_PLACEMENT_3D ( 'NONE', #265, #2684, #7302 ) ;
#4859 = COLOUR_RGB ( '',0.7921568627450980005, 0.8196078431372548767, 0.9333333333333333481 ) ;
#4860 = CIRCLE ( 'NONE', #2512, 23.99999999999999289 ) ;
#4861 = VERTEX_POINT ( 'NONE', #3475 ) ;
#4862 = SHAPE_REPRESENTATION ( 'MAT-051', ( #4494, #201, #5234, #5111, #2288, #4626, #1534, #5850, #2895, #4499, #1786 ), #193 ) ;
#4863 = FACE_OUTER_BOUND ( 'NONE', #3660, .T. ) ;
#4864 = DIRECTION ( 'NONE',  ( -0.7071067811865436870, -8.465450562766819607E-16, 0.7071067811865514585 ) ) ;
#4865 = ADVANCED_FACE ( 'NONE', ( #6891 ), #6398, .F. ) ;
#4866 = ORIENTED_EDGE ( 'NONE', *, *, #3002, .T. ) ;
#4867 = AXIS2_PLACEMENT_3D ( 'NONE', #2655, #6811, #7348 ) ;
#4868 = CARTESIAN_POINT ( 'NONE',  ( 50.00000000000000000, 0.000000000000000000, 35.00000000000000000 ) ) ;
#4869 = TOROIDAL_SURFACE ( 'NONE', #3513, 24.00000000000000000, 3.000000000000000000 ) ;
#4870 = DIRECTION ( 'NONE',  ( 3.081487911019577365E-33, 1.193489751472043281E-15, -1.000000000000000000 ) ) ;
#4871 = VERTEX_POINT ( 'NONE', #6317 ) ;
#4872 = CARTESIAN_POINT ( 'NONE',  ( 209.9999999999999716, 6.000000000000000000, 35.00000000000000000 ) ) ;
#4873 = DIRECTION ( 'NONE',  ( 1.000000000000000000, 0.000000000000000000, 0.000000000000000000 ) ) ;
#4874 = DIRECTION ( 'NONE',  ( 0.000000000000000000, 0.000000000000000000, 1.000000000000000000 ) ) ;
#4875 = DIRECTION ( 'NONE',  ( 0.000000000000000000, 0.000000000000000000, -1.000000000000000000 ) ) ;
#4876 =( LENGTH_UNIT ( ) NAMED_UNIT ( * ) SI_UNIT ( .MILLI., .METRE. ) );
#4877 = EDGE_CURVE ( 'NONE', #4322, #5235, #2659, .T. ) ;
#4878 = EDGE_CURVE ( 'NONE', #1964, #5278, #1119, .T. ) ;
#4879 = CIRCLE ( 'NONE', #6836, 2.999999999999999112 ) ;
#4880 = FACE_OUTER_BOUND ( 'NONE', #390, .T. ) ;
#4881 = FACE_OUTER_BOUND ( 'NONE', #6900, .T. ) ;
#4882 = DIRECTION ( 'NONE',  ( 0.000000000000000000, 0.000000000000000000, -1.000000000000000000 ) ) ;
#4883 = CARTESIAN_POINT ( 'NONE',  ( -60.84172821740799719, -223.0630987092885960, 76.30858369176860379 ) ) ;
#4884 = DIRECTION ( 'NONE',  ( -1.681558157189779738E-44, 0.000000000000000000, -1.000000000000000000 ) ) ;
#4885 = EDGE_CURVE ( 'NONE', #7378, #5359, #4131, .T. ) ;
#4886 = EDGE_LOOP ( 'NONE', ( #2210, #3076, #3718, #3845, #7081, #5735, #4342 ) ) ;
#4887 = ORIENTED_EDGE ( 'NONE', *, *, #1342, .T. ) ;
#4888 = FACE_OUTER_BOUND ( 'NONE', #6370, .T. ) ;
#4889 = AXIS2_PLACEMENT_3D ( 'NONE', #4255, #1320, #668 ) ;
#4890 = LINE ( 'NONE', #3268, #7055 ) ;
#4891 = CARTESIAN_POINT ( 'NONE',  ( 35.00000000000000000, -39.99999999999999289, 0.000000000000000000 ) ) ;
#4892 = CARTESIAN_POINT ( 'NONE',  ( 200.0000000000000000, 0.000000000000000000, 0.000000000000000000 ) ) ;
#4893 = CARTESIAN_POINT ( 'NONE',  ( -53.25168462842736261, -218.0630240738404950, 95.20959099461346398 ) ) ;
#4894 = ORIENTED_EDGE ( 'NONE', *, *, #2073, .T. ) ;
#4895 = ADVANCED_FACE ( 'NONE', ( #3704 ), #6589, .F. ) ;
#4896 = ORIENTED_EDGE ( 'NONE', *, *, #581, .F. ) ;
#4897 = CARTESIAN_POINT ( 'NONE',  ( -24.15685424949240456, -63.34314575050749596, 36.34314575050759544 ) ) ;
#4898 = DIRECTION ( 'NONE',  ( 4.622231866529368100E-33, -2.600005424922769496E-32, 1.000000000000000000 ) ) ;
#4899 = ORIENTED_EDGE ( 'NONE', *, *, #1361, .F. ) ;
#4900 = ITEM_DEFINED_TRANSFORMATION ( 'NONE', 'NONE', #2895,  #1914 ) ;
#4901 = FACE_BOUND ( 'NONE', #1427, .T. ) ;
#4902 = CARTESIAN_POINT ( 'NONE',  ( 24.99999999999999289, 86.00000000000001421, 9.999999999999992895 ) ) ;
#4903 = EDGE_LOOP ( 'NONE', ( #1696, #6444 ) ) ;
#4904 = ADVANCED_FACE ( 'NONE', ( #6621 ), #7421, .T. ) ;
#4905 = CARTESIAN_POINT ( 'NONE',  ( 18.50000000000000711, 101.5000000000000000, 4.999999999999999112 ) ) ;
#4906 = DIRECTION ( 'NONE',  ( 0.000000000000000000, 0.000000000000000000, 1.000000000000000000 ) ) ;
#4907 = ORIENTED_EDGE ( 'NONE', *, *, #4444, .F. ) ;
#4908 = DIRECTION ( 'NONE',  ( -1.000000000000000000, -2.624548829666596736E-30, 9.231085635203017994E-31 ) ) ;
#4909 = DIRECTION ( 'NONE',  ( -0.000000000000000000, 0.000000000000000000, 1.000000000000000000 ) ) ;
#4910 = DIRECTION ( 'NONE',  ( -2.465190328815661892E-32, -0.7071067811865484609, -0.7071067811865465735 ) ) ;
#4911 = ORIENTED_EDGE ( 'NONE', *, *, #7361, .T. ) ;
#4912 = VERTEX_POINT ( 'NONE', #2465 ) ;
#4913 = CARTESIAN_POINT ( 'NONE',  ( 25.00000000000000711, 28.00000000000002487, 9.999999999999996447 ) ) ;
#4914 = SURFACE_STYLE_FILL_AREA ( #2560 ) ;
#4915 = CARTESIAN_POINT ( 'NONE',  ( 217.0000000000000000, -56.99999999999999289, 5.510910596163094486E-16 ) ) ;
#4916 = DIRECTION ( 'NONE',  ( -1.000000000000000000, 5.551115123125783935E-17, -4.237045877651919561E-33 ) ) ;
#4917 = EDGE_CURVE ( 'NONE', #5074, #6069, #4601, .T. ) ;
#4918 = DIRECTION ( 'NONE',  ( -1.000000000000000000, 4.067564042545842122E-31, -3.379803290564626122E-16 ) ) ;
#4919 = ORIENTED_EDGE ( 'NONE', *, *, #5550, .T. ) ;
#4920 = LINE ( 'NONE', #7258, #3577 ) ;
#4921 = VERTEX_POINT ( 'NONE', #6553 ) ;
#4922 = ORIENTED_EDGE ( 'NONE', *, *, #5038, .F. ) ;
#4923 = CARTESIAN_POINT ( 'NONE',  ( -53.10580595754475297, -219.7017882839731158, 72.38063772785491778 ) ) ;
#4924 = CARTESIAN_POINT ( 'NONE',  ( 4.000000000000000000, 0.000000000000000000, 0.000000000000000000 ) ) ;
#4925 = CIRCLE ( 'NONE', #369, 26.99999999999999289 ) ;
#4926 = CIRCLE ( 'NONE', #2582, 13.99999999999999645 ) ;
#4927 = DIRECTION ( 'NONE',  ( -9.244463733058732095E-33, -5.551115123125783935E-17, 1.000000000000000000 ) ) ;
#4928 =( NAMED_UNIT ( * ) PLANE_ANGLE_UNIT ( ) SI_UNIT ( $, .RADIAN. ) );
#4929 = CARTESIAN_POINT ( 'NONE',  ( -61.30885008117680712, -218.0630240738405519, 91.74137814073138486 ) ) ;
#4930 = ORIENTED_EDGE ( 'NONE', *, *, #4885, .T. ) ;
#4931 = EDGE_LOOP ( 'NONE', ( #4644, #7354, #3440, #5771 ) ) ;
#4932 = EDGE_CURVE ( 'NONE', #3769, #734, #3633, .T. ) ;
#4933 = CYLINDRICAL_SURFACE ( 'NONE', #52, 25.00000000000000000 ) ;
#4934 = DIRECTION ( 'NONE',  ( 0.000000000000000000, 0.000000000000000000, -1.000000000000000000 ) ) ;
#4935 = ORIENTED_EDGE ( 'NONE', *, *, #2870, .F. ) ;
#4936 = ITEM_DEFINED_TRANSFORMATION ( 'NONE', 'NONE', #1786,  #1914 ) ;
#4937 = AXIS2_PLACEMENT_3D ( 'NONE', #2848, #5239, #497 ) ;
#4938 = ADVANCED_FACE ( 'NONE', ( #3670 ), #4113, .T. ) ;
#4939 = LINE ( 'NONE', #313, #7139 ) ;
#4940 = DIRECTION ( 'NONE',  ( -1.078147950931789757E-16, 0.000000000000000000, 1.000000000000000000 ) ) ;
#4941 = ORIENTED_EDGE ( 'NONE', *, *, #2032, .T. ) ;
#4942 = AXIS2_PLACEMENT_3D ( 'NONE', #4694, #7029, #1363 ) ;
#4943 = DIRECTION ( 'NONE',  ( 0.000000000000000000, 0.000000000000000000, 1.000000000000000000 ) ) ;
#4944 = CARTESIAN_POINT ( 'NONE',  ( 52.84383605862925748, 25.58527333940346082, 10.00000000000000888 ) ) ;
#4945 = CARTESIAN_POINT ( 'NONE',  ( 217.0000000000000000, -60.00000000000000000, 0.000000000000000000 ) ) ;
#4946 = EDGE_LOOP ( 'NONE', ( #6013, #4116, #5958, #5618 ) ) ;
#4947 = AXIS2_PLACEMENT_3D ( 'NONE', #1453, #6730, #954 ) ;
#4948 = DIRECTION ( 'NONE',  ( 0.000000000000000000, 0.000000000000000000, -1.000000000000000000 ) ) ;
#4949 = EDGE_CURVE ( 'NONE', #7465, #510, #1343, .T. ) ;
#4950 = LINE ( 'NONE', #5600, #1849 ) ;
#4951 = EDGE_CURVE ( 'NONE', #4160, #1940, #413, .T. ) ;
#4952 = LINE ( 'NONE', #7286, #5162 ) ;
#4953 = ORIENTED_EDGE ( 'NONE', *, *, #6739, .T. ) ;
#4954 = DIRECTION ( 'NONE',  ( 4.336808689942013792E-16, 0.000000000000000000, 1.000000000000000000 ) ) ;
#4955 = CARTESIAN_POINT ( 'NONE',  ( 36.00000000000000000, 7.347880794884120722E-16, -5.999999999999986677 ) ) ;
#4956 = CARTESIAN_POINT ( 'NONE',  ( -61.15513345216592000, -223.0630249525806903, 76.61458237095268942 ) ) ;
#4957 = VERTEX_POINT ( 'NONE', #6476 ) ;
#4958 = DIRECTION ( 'NONE',  ( -0.000000000000000000, 1.000000000000000000, 2.065146995210484941E-16 ) ) ;
#4959 = ORIENTED_EDGE ( 'NONE', *, *, #6801, .F. ) ;
#4960 = ORIENTED_EDGE ( 'NONE', *, *, #1434, .F. ) ;
#4961 = CARTESIAN_POINT ( 'NONE',  ( 220.0000000000000000, -60.00000000000000000, 3.000000000000000888 ) ) ;
#4962 = DIRECTION ( 'NONE',  ( 0.000000000000000000, 0.000000000000000000, -1.000000000000000000 ) ) ;
#4963 = DIRECTION ( 'NONE',  ( 0.000000000000000000, 0.000000000000000000, -1.000000000000000000 ) ) ;
#4964 = AXIS2_PLACEMENT_3D ( 'NONE', #6204, #2093, #3326 ) ;
#4965 = FACE_OUTER_BOUND ( 'NONE', #2302, .T. ) ;
#4966 = AXIS2_PLACEMENT_3D ( 'NONE', #2674, #3334, #6792 ) ;
#4967 = ORIENTED_EDGE ( 'NONE', *, *, #1617, .T. ) ;
#4968 = EDGE_CURVE ( 'NONE', #3465, #2464, #699, .T. ) ;
#4969 = ORIENTED_EDGE ( 'NONE', *, *, #1905, .F. ) ;
#4970 = VECTOR ( 'NONE', #842, 999.9999999999998863 ) ;
#4971 = AXIS2_PLACEMENT_3D ( 'NONE', #5264, #4804, #4153 ) ;
#4972 = CARTESIAN_POINT ( 'NONE',  ( -26.50000000000003197, -60.68629150101524772, -11.31370849898474873 ) ) ;
#4973 = DIRECTION ( 'NONE',  ( -1.681558157189779489E-44, 0.000000000000000000, -1.000000000000000000 ) ) ;
#4974 = ORIENTED_EDGE ( 'NONE', *, *, #4334, .T. ) ;
#4975 = DIRECTION ( 'NONE',  ( 1.000000000000000000, 0.000000000000000000, -5.605193857299270773E-45 ) ) ;
#4976 = CARTESIAN_POINT ( 'NONE',  ( -16.49999999999998579, -125.0933926253236308, 30.46597562735434295 ) ) ;
#4977 = AXIS2_PLACEMENT_3D ( 'NONE', #1962, #2115, #4464 ) ;
#4978 = PRESENTATION_LAYER_ASSIGNMENT (  '', '', ( #5588 ) ) ;
#4979 = CONICAL_SURFACE ( 'NONE', #6576, 9.999999999999998224, 0.7853981633974501664 ) ;
#4980 = ORIENTED_EDGE ( 'NONE', *, *, #5920, .T. ) ;
#4981 = ADVANCED_FACE ( 'NONE', ( #4863 ), #1818, .T. ) ;
#4982 = CARTESIAN_POINT ( 'NONE',  ( 24.99999999999999289, 86.00000000000001421, 4.999999999999992006 ) ) ;
#4983 = AXIS2_PLACEMENT_3D ( 'NONE', #6916, #3888, #2718 ) ;
#4984 = AXIS2_PLACEMENT_3D ( 'NONE', #5816, #4167, #2888 ) ;
#4985 = DIRECTION ( 'NONE',  ( 0.000000000000000000, 0.000000000000000000, 1.000000000000000000 ) ) ;
#4986 = CARTESIAN_POINT ( 'NONE',  ( -24.81370849898475939, -223.0630240738404382, 73.28127814332046341 ) ) ;
#4987 = CIRCLE ( 'NONE', #1907, 10.00000000000001954 ) ;
#4988 = ORIENTED_EDGE ( 'NONE', *, *, #5736, .F. ) ;
#4989 =( NAMED_UNIT ( * ) SI_UNIT ( $, .STERADIAN. ) SOLID_ANGLE_UNIT ( ) );
#4990 = DIRECTION ( 'NONE',  ( -1.000000000000000000, 5.551115123125783935E-17, -4.237045877651919561E-33 ) ) ;
#4991 = CARTESIAN_POINT ( 'NONE',  ( 25.00000000000000711, 40.21320343559642652, 5.999999999999996447 ) ) ;
#4992 = CARTESIAN_POINT ( 'NONE',  ( 220.0000000000000000, -9.000000000000001776, 18.00000000000001066 ) ) ;
#4993 = ORIENTED_EDGE ( 'NONE', *, *, #4653, .T. ) ;
#4994 = ORIENTED_EDGE ( 'NONE', *, *, #2468, .F. ) ;
#4995 = EDGE_CURVE ( 'NONE', #1465, #4834, #2741, .T. ) ;
#4996 = DIRECTION ( 'NONE',  ( -1.000000000000000000, 0.000000000000000000, 0.000000000000000000 ) ) ;
#4997 = PRESENTATION_STYLE_ASSIGNMENT (( #3142 ) ) ;
#4998 = DIRECTION ( 'NONE',  ( 0.000000000000000000, 0.000000000000000000, 1.000000000000000000 ) ) ;
#4999 = CARTESIAN_POINT ( 'NONE',  ( -63.60023158588590064, -223.0630242615051202, 80.29653509657342170 ) ) ;
#5000 = CARTESIAN_POINT ( 'NONE',  ( 188.6380400399839061, -9.000000000000001776, 15.00000000000000888 ) ) ;
#5001 = CARTESIAN_POINT ( 'NONE',  ( 25.00000000000000711, 77.32233047033632545, 4.535533905932710219 ) ) ;
#5002 = VERTEX_POINT ( 'NONE', #4713 ) ;
#5003 = EDGE_CURVE ( 'NONE', #5285, #5929, #1852, .T. ) ;
#5004 = EDGE_CURVE ( 'NONE', #3862, #3547, #3325, .T. ) ;
#5005 = EDGE_LOOP ( 'NONE', ( #1213, #2651, #6283, #1063, #6483, #1480, #691, #5571 ) ) ;
#5006 = CARTESIAN_POINT ( 'NONE',  ( -21.50000000000000000, -120.9522879036833558, 45.92078884797942351 ) ) ;
#5007 = DIRECTION ( 'NONE',  ( 0.000000000000000000, 0.000000000000000000, -1.000000000000000000 ) ) ;
#5008 = FACE_OUTER_BOUND ( 'NONE', #830, .T. ) ;
#5009 = AXIS2_PLACEMENT_3D ( 'NONE', #5025, #7288, #6749 ) ;
#5010 = EDGE_LOOP ( 'NONE', ( #1322, #4739, #3869, #6380 ) ) ;
#5011 = ORIENTED_EDGE ( 'NONE', *, *, #1072, .T. ) ;
#5012 = AXIS2_PLACEMENT_3D ( 'NONE', #7240, #318, #279 ) ;
#5013 = DIRECTION ( 'NONE',  ( 2.465190328815662439E-32, 0.7071067811865465735, -0.7071067811865485719 ) ) ;
#5014 = ORIENTED_EDGE ( 'NONE', *, *, #993, .F. ) ;
#5015 = EDGE_CURVE ( 'NONE', #5534, #2796, #296, .T. ) ;
#5016 = DIRECTION ( 'NONE',  ( 0.000000000000000000, -0.03489949670250429292, -0.9993908270190955401 ) ) ;
#5017 = ORIENTED_EDGE ( 'NONE', *, *, #3884, .T. ) ;
#5018 = FACE_OUTER_BOUND ( 'NONE', #2985, .T. ) ;
#5019 = CARTESIAN_POINT ( 'NONE',  ( -21.49999999999999645, -219.7493155748557285, 72.39337262706536080 ) ) ;
#5020 = VERTEX_POINT ( 'NONE', #1234 ) ;
#5021 = CARTESIAN_POINT ( 'NONE',  ( -53.17910001414513488, -216.4242598635583477, 94.92063264932129130 ) ) ;
#5022 = FACE_OUTER_BOUND ( 'NONE', #5423, .T. ) ;
#5023 = CARTESIAN_POINT ( 'NONE',  ( 36.00000000000000000, 0.000000000000000000, 6.000000000000015099 ) ) ;
#5024 = ORIENTED_EDGE ( 'NONE', *, *, #4377, .T. ) ;
#5025 = CARTESIAN_POINT ( 'NONE',  ( 35.00000000000000000, 39.99999999999999289, 0.000000000000000000 ) ) ;
#5026 = CARTESIAN_POINT ( 'NONE',  ( 2.000000000000001776, 1.224646799147405913E-15, -9.999999999999998224 ) ) ;
#5027 = CARTESIAN_POINT ( 'NONE',  ( 50.00000000000000000, 0.000000000000000000, 48.99999999999999289 ) ) ;
#5028 = CARTESIAN_POINT ( 'NONE',  ( -60.84337381445615733, -223.0630240738404950, 93.24745791952346963 ) ) ;
#5029 = FACE_OUTER_BOUND ( 'NONE', #7039, .T. ) ;
#5030 = CARTESIAN_POINT ( 'NONE',  ( 0.000000000000000000, 0.000000000000000000, -39.99999999999997868 ) ) ;
#5031 = ADVANCED_FACE ( 'NONE', ( #5361, #92 ), #2432, .F. ) ;
#5032 = EDGE_LOOP ( 'NONE', ( #2289, #2068 ) ) ;
#5033 = VERTEX_POINT ( 'NONE', #129 ) ;
#5034 = CARTESIAN_POINT ( 'NONE',  ( -24.81370849898475583, -223.0630240738404382, 96.09122589815579829 ) ) ;
#5035 = DIRECTION ( 'NONE',  ( -7.663350976776344912E-46, 0.000000000000000000, -1.000000000000000000 ) ) ;
#5036 = FACE_OUTER_BOUND ( 'NONE', #5279, .T. ) ;
#5037 = FACE_OUTER_BOUND ( 'NONE', #2310, .T. ) ;
#5038 = EDGE_CURVE ( 'NONE', #687, #2809, #2197, .T. ) ;
#5039 = CIRCLE ( 'NONE', #1714, 10.00000000000000355 ) ;
#5040 = ORIENTED_EDGE ( 'NONE', *, *, #7155, .T. ) ;
#5041 = ORIENTED_EDGE ( 'NONE', *, *, #2114, .T. ) ;
#5042 = VECTOR ( 'NONE', #116, 999.9999999999998863 ) ;
#5043 = CARTESIAN_POINT ( 'NONE',  ( 0.000000000000000000, -23.20733648494241663, 0.8104180479081783961 ) ) ;
#5044 = ORIENTED_EDGE ( 'NONE', *, *, #4508, .F. ) ;
#5045 = DIRECTION ( 'NONE',  ( 0.000000000000000000, 0.000000000000000000, -1.000000000000000000 ) ) ;
#5046 = CARTESIAN_POINT ( 'NONE',  ( -21.50563895418471461, -113.9621117585880512, 41.96211175858820042 ) ) ;
#5047 = VECTOR ( 'NONE', #7474, 1000.000000000000000 ) ;
#5048 = VERTEX_POINT ( 'NONE', #4897 ) ;
#5049 = FACE_OUTER_BOUND ( 'NONE', #4633, .T. ) ;
#5050 = CARTESIAN_POINT ( 'NONE',  ( -29.50000000000000000, -223.0630240738404950, 73.28127814332044920 ) ) ;
#5051 = ORIENTED_EDGE ( 'NONE', *, *, #7577, .F. ) ;
#5052 = CARTESIAN_POINT ( 'NONE',  ( -61.04530230988101636, 7.783800328198303619E-27, 35.00000000000000000 ) ) ;
#5053 = CARTESIAN_POINT ( 'NONE',  ( -53.01709100512436379, -212.7665347604136912, 94.27567702562228646 ) ) ;
#5054 = CARTESIAN_POINT ( 'NONE',  ( 220.0000000000000000, 56.99999999999999289, 3.000000000000021316 ) ) ;
#5055 = VERTEX_POINT ( 'NONE', #7312 ) ;
#5056 = PRODUCT ( 'connecting rod', 'connecting rod', '', ( #10 ) ) ;
#5057 = ORIENTED_EDGE ( 'NONE', *, *, #5945, .F. ) ;
#5058 = EDGE_CURVE ( 'NONE', #2795, #3993, #6734, .T. ) ;
#5059 = CARTESIAN_POINT ( 'NONE',  ( 193.5000000000000000, 39.99999999999999289, 0.000000000000000000 ) ) ;
#5060 =( NAMED_UNIT ( * ) SI_UNIT ( $, .STERADIAN. ) SOLID_ANGLE_UNIT ( ) );
#5061 = CARTESIAN_POINT ( 'NONE',  ( 47.00000000000000000, -21.98659819442010388, 35.76778892745510063 ) ) ;
#5062 = CARTESIAN_POINT ( 'NONE',  ( -61.57753664718645581, -223.0629867915132536, 92.46999602602490143 ) ) ;
#5063 = FACE_OUTER_BOUND ( 'NONE', #7471, .T. ) ;
#5064 = CARTESIAN_POINT ( 'NONE',  ( 188.6380400399839061, 9.000000000000001776, 15.00000000000000888 ) ) ;
#5065 = CARTESIAN_POINT ( 'NONE',  ( -57.45460281882250797, -218.0630240738404666, 72.85609881942959021 ) ) ;
#5066 = VECTOR ( 'NONE', #6895, 1000.000000000000000 ) ;
#5067 = EDGE_LOOP ( 'NONE', ( #1582, #3883, #6387, #2804 ) ) ;
#5068 = ADVANCED_FACE ( 'NONE', ( #5583 ), #4933, .T. ) ;
#5069 = ORIENTED_EDGE ( 'NONE', *, *, #6596, .F. ) ;
#5070 = LINE ( 'NONE', #6298, #5832 ) ;
#5071 = CARTESIAN_POINT ( 'NONE',  ( -29.49999999999998934, 16.00000000000004263, 42.31370849898485886 ) ) ;
#5072 = CARTESIAN_POINT ( 'NONE',  ( 3.000000000000002665, -60.00000000000000000, 7.000000000000000888 ) ) ;
#5073 = CYLINDRICAL_SURFACE ( 'NONE', #760, 9.999999999999996447 ) ;
#5074 = VERTEX_POINT ( 'NONE', #6118 ) ;
#5075 = ORIENTED_EDGE ( 'NONE', *, *, #181, .T. ) ;
#5076 = EDGE_CURVE ( 'NONE', #4326, #551, #236, .T. ) ;
#5077 = EDGE_CURVE ( 'NONE', #6591, #2069, #3275, .T. ) ;
#5078 = DIRECTION ( 'NONE',  ( 0.000000000000000000, -1.000000000000000000, -0.000000000000000000 ) ) ;
#5079 = ORIENTED_EDGE ( 'NONE', *, *, #6363, .F. ) ;
#5080 = CARTESIAN_POINT ( 'NONE',  ( 220.0000000000000000, -15.08392021690038298, 15.00000000000000888 ) ) ;
#5081 = CYLINDRICAL_SURFACE ( 'NONE', #4867, 6.000000000000001776 ) ;
#5082 = ORIENTED_EDGE ( 'NONE', *, *, #1521, .F. ) ;
#5083 = AXIS2_PLACEMENT_3D ( 'NONE', #7089, #3554, #4824 ) ;
#5084 = CIRCLE ( 'NONE', #43, 2.999999999999999556 ) ;
#5085 = EDGE_CURVE ( 'NONE', #5661, #4957, #1830, .T. ) ;
#5086 = ADVANCED_FACE ( 'NONE', ( #272, #5544 ), #3894, .T. ) ;
#5087 = CARTESIAN_POINT ( 'NONE',  ( 49.52414331456670027, 25.96382905951872644, 9.999999999999324984 ) ) ;
#5088 = FACE_OUTER_BOUND ( 'NONE', #3355, .T. ) ;
#5089 = ORIENTED_EDGE ( 'NONE', *, *, #3893, .F. ) ;
#5090 =( LENGTH_UNIT ( ) NAMED_UNIT ( * ) SI_UNIT ( .MILLI., .METRE. ) );
#5091 = VECTOR ( 'NONE', #2999, 1000.000000000000000 ) ;
#5092 = CARTESIAN_POINT ( 'NONE',  ( -52.98766809822284785, -212.1022451272887110, 94.15854484029739524 ) ) ;
#5093 = AXIS2_PLACEMENT_3D ( 'NONE', #71, #1799, #6989 ) ;
#5094 = FACE_OUTER_BOUND ( 'NONE', #2687, .T. ) ;
#5095 = AXIS2_PLACEMENT_3D ( 'NONE', #213, #2554, #4873 ) ;
#5096 = CARTESIAN_POINT ( 'NONE',  ( 0.000000000000000000, -21.98659819442010388, 35.76778892745510063 ) ) ;
#5097 = ORIENTED_EDGE ( 'NONE', *, *, #2448, .T. ) ;
#5098 = ORIENTED_EDGE ( 'NONE', *, *, #6607, .F. ) ;
#5099 = AXIS2_PLACEMENT_3D ( 'NONE', #608, #3140, #690 ) ;
#5100 = ADVANCED_BREP_SHAPE_REPRESENTATION ( '', ( #6388, #1914 ), #7073 ) ;
#5101 = CIRCLE ( 'NONE', #2276, 14.00000000000000533 ) ;
#5102 = CIRCLE ( 'NONE', #428, 3.000000000000000000 ) ;
#5103 =( BOUNDED_CURVE ( )  B_SPLINE_CURVE ( 3, ( #965, #2049, #4404, #4516 ),
 .UNSPECIFIED., .F., .T. ) 
 B_SPLINE_CURVE_WITH_KNOTS ( ( 4, 4 ),
 ( 3.141592653589793116, 6.283185307179586232 ),
 .UNSPECIFIED. ) 
 CURVE ( )  GEOMETRIC_REPRESENTATION_ITEM ( )  RATIONAL_B_SPLINE_CURVE ( ( 1.000000000000000000, 0.3333333333333333703, 0.3333333333333333703, 1.000000000000000000 ) ) 
 REPRESENTATION_ITEM ( '' )  );
#5104 = DIRECTION ( 'NONE',  ( -0.6427876096865581257, 9.159339953157541458E-16, -0.7660444431189622483 ) ) ;
#5105 = DIRECTION ( 'NONE',  ( 0.000000000000000000, 0.000000000000000000, -1.000000000000000000 ) ) ;
#5106 = CARTESIAN_POINT ( 'NONE',  ( -63.72956387582338778, -223.0630239280731928, 88.95744984476777972 ) ) ;
#5107 = CARTESIAN_POINT ( 'NONE',  ( 3.000000000000002665, 56.99999999999999289, 10.00000000000002132 ) ) ;
#5108 = CARTESIAN_POINT ( 'NONE',  ( 26.00000000000000000, 1.224646799147344973E-15, -9.999999999999998224 ) ) ;
#5109 = EDGE_CURVE ( 'NONE', #2578, #1052, #2576, .T. ) ;
#5110 = CIRCLE ( 'NONE', #2889, 8.500000000000007105 ) ;
#5112 = CARTESIAN_POINT ( 'NONE',  ( -32.50000000000002842, -60.68629150101523351, -11.31370849898474873 ) ) ;
#5111 = AXIS2_PLACEMENT_3D ( 'NONE', #6781, #1540, #5667 ) ;
#5113 = VERTEX_POINT ( 'NONE', #2689 ) ;
#5114 = ORIENTED_EDGE ( 'NONE', *, *, #2636, .F. ) ;
#5115 = CARTESIAN_POINT ( 'NONE',  ( 188.0000000000000000, 11.00000000000000533, 0.000000000000000000 ) ) ;
#5116 = LINE ( 'NONE', #299, #4507 ) ;
#5117 = DIRECTION ( 'NONE',  ( -0.6444004775717538935, -0.5407162030609466985, 0.5407162030609482528 ) ) ;
#5118 = CARTESIAN_POINT ( 'NONE',  ( 170.0000000000000000, -10.56957438397690474, -9.180637088000993984 ) ) ;
#5119 = LINE ( 'NONE', #6917, #1128 ) ;
#5120 = EDGE_LOOP ( 'NONE', ( #5451, #2721, #342, #7298 ) ) ;
#5121 = EDGE_LOOP ( 'NONE', ( #3710, #972, #5997, #4820 ) ) ;
#5122 = CYLINDRICAL_SURFACE ( 'NONE', #3255, 10.00000000000001954 ) ;
#5123 = EDGE_LOOP ( 'NONE', ( #2552, #4045 ) ) ;
#5124 = CARTESIAN_POINT ( 'NONE',  ( 50.68728032241775594, -27.58259254939923721, 10.00000000000000533 ) ) ;
#5125 = CARTESIAN_POINT ( 'NONE',  ( 50.29734716306172970, -18.29734716306171549, 10.98910980934740778 ) ) ;
#5126 = EDGE_CURVE ( 'NONE', #1438, #6974, #5947, .T. ) ;
#5127 = EDGE_LOOP ( 'NONE', ( #1918, #1032, #357, #6848 ) ) ;
#5128 = LINE ( 'NONE', #3359, #539 ) ;
#5129 = DIRECTION ( 'NONE',  ( 1.000000000000000000, 0.000000000000000000, 0.000000000000000000 ) ) ;
#5130 = ORIENTED_EDGE ( 'NONE', *, *, #7595, .F. ) ;
#5131 = VECTOR ( 'NONE', #4647, 1000.000000000000000 ) ;
#5132 = CARTESIAN_POINT ( 'NONE',  ( -53.06880420804608889, -213.9340789708228954, 94.48154657108737808 ) ) ;
#5133 = CARTESIAN_POINT ( 'NONE',  ( -32.50000000000002132, -45.34314575050759544, 18.34314575050763452 ) ) ;
#5134 = CYLINDRICAL_SURFACE ( 'NONE', #1385, 3.000000000000007994 ) ;
#5135 = ORIENTED_EDGE ( 'NONE', *, *, #6060, .F. ) ;
#5136 = EDGE_CURVE ( 'NONE', #4506, #162, #1893, .T. ) ;
#5137 = ORIENTED_EDGE ( 'NONE', *, *, #5605, .F. ) ;
#5138 = EDGE_CURVE ( 'NONE', #4666, #7513, #2001, .T. ) ;
#5139 = PLANE ( 'NONE',  #4272 ) ;
#5140 = CARTESIAN_POINT ( 'NONE',  ( 25.00000000000002132, 28.00000000000002487, 0.000000000000000000 ) ) ;
#5141 = CARTESIAN_POINT ( 'NONE',  ( -26.50000000000000711, -71.76505905230354188, 44.76505905230365556 ) ) ;
#5142 = CARTESIAN_POINT ( 'NONE',  ( 4.000000000000000000, 0.000000000000000000, 0.000000000000000000 ) ) ;
#5143 = LINE ( 'NONE', #6412, #7250 ) ;
#5144 = DIRECTION ( 'NONE',  ( 4.622231866529368100E-33, -2.600005424922769496E-32, 1.000000000000000000 ) ) ;
#5145 = CARTESIAN_POINT ( 'NONE',  ( -64.34713424250860214, -218.0649563631192223, 81.64184023509517374 ) ) ;
#5146 =( BOUNDED_SURFACE ( )  B_SPLINE_SURFACE ( 5, 3, ( 
 ( #1157, #2287, #7583, #543, #6514, #1661, #4132, #2320, #7045, #2392, #7542, #4756, #6437, #5203, #1736, #3595 ),
 ( #1195, #5894, #621, #2970, #2894, #3518, #3442, #5861, #7090, #4171, #5317, #2246, #5783, #4637, #583, #5245 ),
 ( #1235, #504, #6365, #2854, #4673, #2814, #5166, #3476, #7506, #4592, #6976, #6399, #7010, #2929, #7, #2356 ),
 ( #4714, #7273, #206, #2002, #130, #4209, #3121, #4247, #2505, #1888, #237, #3055, #3781, #1931, #700, #733 ),
 ( #5399, #3743, #7200, #6047, #1380, #2466, #1853, #93, #6590, #5512, #6554, #4356, #4790, #2433, #1313, #4281 ),
 ( #6698, #7161, #661, #4825, #3012, #2547, #3671, #7124, #6009, #6658, #164, #1273, #6084, #809, #1424, #3089 ) ),
 .UNSPECIFIED., .F., .F., .T. ) 
 B_SPLINE_SURFACE_WITH_KNOTS ( ( 6, 6 ),
 ( 4, 2, 2, 2, 2, 2, 2, 4 ),
 ( 0.000000000000000000, 1.000000000000000000 ),
 ( -1.150125124083905659, -0.9546592037126467867, -0.4819498650540673390, 0.000000000000000000, 0.02616758540912784634, 0.5083707369372295615, 0.9999999999999414912, 1.195465920371200363 ),
 .UNSPECIFIED. ) 
 GEOMETRIC_REPRESENTATION_ITEM ( )  RATIONAL_B_SPLINE_SURFACE ( (
 ( 1.000000000000000000, 1.000000000000000000, 1.000000000000000000, 1.000000000000000000, 1.000000000000000000, 1.000000000000000000, 1.000000000000000000, 1.000000000000000000, 1.000000000000000000, 1.000000000000000000, 1.000000000000000000, 1.000000000000000000, 1.000000000000000000, 1.000000000000000000, 1.000000000000000000, 1.000000000000000000),
 ( 0.5999999999999995337, 0.5999999999999995337, 0.5999999999999999778, 0.5999999999999999778, 0.5999999999999999778, 0.5999999999999999778, 0.5999999999999999778, 0.5999999999999999778, 0.5999999999999995337, 0.5999999999999995337, 0.5999999999999999778, 0.5999999999999999778, 0.5999999999999989786, 0.5999999999999989786, 0.5999999999999995337, 0.5999999999999995337),
 ( 0.3999999999999993561, 0.3999999999999993561, 0.4000000000000000777, 0.4000000000000000777, 0.4000000000000000777, 0.4000000000000000777, 0.4000000000000000777, 0.4000000000000000777, 0.3999999999999993561, 0.3999999999999993561, 0.4000000000000000777, 0.4000000000000000777, 0.3999999999999984679, 0.3999999999999984679, 0.3999999999999993561, 0.3999999999999993561),
 ( 0.3999999999999993561, 0.3999999999999993561, 0.4000000000000000777, 0.4000000000000000777, 0.4000000000000000777, 0.4000000000000000777, 0.4000000000000000777, 0.4000000000000000777, 0.3999999999999993561, 0.3999999999999993561, 0.4000000000000000777, 0.4000000000000000777, 0.3999999999999984679, 0.3999999999999984679, 0.3999999999999993561, 0.3999999999999993561),
 ( 0.5999999999999995337, 0.5999999999999995337, 0.5999999999999999778, 0.5999999999999999778, 0.5999999999999999778, 0.5999999999999999778, 0.5999999999999999778, 0.5999999999999999778, 0.5999999999999995337, 0.5999999999999995337, 0.5999999999999999778, 0.5999999999999999778, 0.5999999999999989786, 0.5999999999999989786, 0.5999999999999995337, 0.5999999999999995337),
 ( 1.000000000000000000, 1.000000000000000000, 1.000000000000000000, 1.000000000000000000, 1.000000000000000000, 1.000000000000000000, 1.000000000000000000, 1.000000000000000000, 1.000000000000000000, 1.000000000000000000, 1.000000000000000000, 1.000000000000000000, 1.000000000000000000, 1.000000000000000000, 1.000000000000000000, 1.000000000000000000) ) ) 
 REPRESENTATION_ITEM ( '' )  SURFACE ( )  );
#5147 = ORIENTED_EDGE ( 'NONE', *, *, #3942, .F. ) ;
#5148 = ORIENTED_EDGE ( 'NONE', *, *, #3314, .F. ) ;
#5149 = ADVANCED_FACE ( 'NONE', ( #4316 ), #58, .T. ) ;
#5150 = DIRECTION ( 'NONE',  ( 0.000000000000000000, 0.000000000000000000, 1.000000000000000000 ) ) ;
#5151 = DIRECTION ( 'NONE',  ( 1.000000000000000000, 1.853902270198408060E-44, 1.681558157189780485E-44 ) ) ;
#5152 = DIRECTION ( 'NONE',  ( 1.000000000000000000, 0.000000000000000000, 0.000000000000000000 ) ) ;
#5153 = CARTESIAN_POINT ( 'NONE',  ( -16.49999999999998934, -71.76505905230354188, 44.76505905230365556 ) ) ;
#5154 = VERTEX_POINT ( 'NONE', #3234 ) ;
#5155 = ORIENTED_EDGE ( 'NONE', *, *, #1775, .F. ) ;
#5156 = LINE ( 'NONE', #6053, #7580 ) ;
#5157 = DIRECTION ( 'NONE',  ( 1.000000000000000000, 1.853902270198408060E-44, -1.681558157189779738E-44 ) ) ;
#5158 = CARTESIAN_POINT ( 'NONE',  ( 3.000000000000002665, 24.90486745229362953, 37.17889356869155648 ) ) ;
#5159 = CARTESIAN_POINT ( 'NONE',  ( 12.50000000000000355, 101.5000000000000000, 4.999999999999999112 ) ) ;
#5160 = ORIENTED_EDGE ( 'NONE', *, *, #4082, .F. ) ;
#5161 = AXIS2_PLACEMENT_3D ( 'NONE', #108, #1976, #5375 ) ;
#5162 = VECTOR ( 'NONE', #4375, 1000.000000000000000 ) ;
#5163 = EDGE_CURVE ( 'NONE', #1140, #2192, #2612, .T. ) ;
#5164 = EDGE_CURVE ( 'NONE', #208, #2155, #7345, .T. ) ;
#5165 = FACE_OUTER_BOUND ( 'NONE', #1135, .T. ) ;
#5166 = CARTESIAN_POINT ( 'NONE',  ( 27.10306686690893940, -220.2280969603149003, 89.90726370123081779 ) ) ;
#5167 = ORIENTED_EDGE ( 'NONE', *, *, #3954, .F. ) ;
#5168 = CARTESIAN_POINT ( 'NONE',  ( 3.000000000000002665, -22.78897920707096247, 12.79060301978498160 ) ) ;
#5169 = AXIS2_PLACEMENT_3D ( 'NONE', #6592, #3558, #2398 ) ;
#5170 = DIRECTION ( 'NONE',  ( 0.000000000000000000, 0.000000000000000000, 1.000000000000000000 ) ) ;
#5171 = PLANE ( 'NONE',  #2993 ) ;
#5172 = ORIENTED_EDGE ( 'NONE', *, *, #7157, .T. ) ;
#5173 = ORIENTED_EDGE ( 'NONE', *, *, #3395, .T. ) ;
#5174 = AXIS2_PLACEMENT_3D ( 'NONE', #5815, #1694, #1149 ) ;
#5175 = DIRECTION ( 'NONE',  ( 0.000000000000000000, 0.000000000000000000, 1.000000000000000000 ) ) ;
#5176 = EDGE_CURVE ( 'NONE', #3850, #208, #3578, .T. ) ;
#5177 = EDGE_CURVE ( 'NONE', #6636, #2714, #3007, .T. ) ;
#5178 = CARTESIAN_POINT ( 'NONE',  ( 187.9839735574547603, 6.029117148349426358, 16.86712362072634264 ) ) ;
#5179 = CYLINDRICAL_SURFACE ( 'NONE', #6311, 15.99999999999999645 ) ;
#5180 = LINE ( 'NONE', #3529, #3696 ) ;
#5181 = DIRECTION ( 'NONE',  ( 1.853902270198407313E-44, 1.000000000000000000, 0.000000000000000000 ) ) ;
#5182 = PRODUCT_RELATED_PRODUCT_CATEGORY ( 'part', '', ( #3046 ) ) ;
#5183 = COLOUR_RGB ( '',0.7921568627450980005, 0.8196078431372548767, 0.9333333333333333481 ) ;
#5184 = CARTESIAN_POINT ( 'NONE',  ( -59.96426363863164255, -218.0635656269040510, 74.31118017701729173 ) ) ;
#5185 = UNCERTAINTY_MEASURE_WITH_UNIT (LENGTH_MEASURE( 1.000000000000000082E-05 ), #4108, 'distance_accuracy_value', 'NONE');
#5186 = ORIENTED_EDGE ( 'NONE', *, *, #3233, .T. ) ;
#5187 = CARTESIAN_POINT ( 'NONE',  ( 0.000000000000000000, 0.000000000000000000, 0.000000000000000000 ) ) ;
#5188 = CARTESIAN_POINT ( 'NONE',  ( 36.00000000000000000, 0.000000000000000000, 1.387778780781445676E-14 ) ) ;
#5189 = DIRECTION ( 'NONE',  ( 0.000000000000000000, -0.000000000000000000, -1.000000000000000000 ) ) ;
#5190 = CYLINDRICAL_SURFACE ( 'NONE', #2395, 8.500000000000007105 ) ;
#5191 = CARTESIAN_POINT ( 'NONE',  ( 186.0399638286305901, -9.000000000000001776, 13.50000000000000178 ) ) ;
#5192 = ORIENTED_EDGE ( 'NONE', *, *, #6532, .T. ) ;
#5193 = EDGE_LOOP ( 'NONE', ( #4097, #6319 ) ) ;
#5194 = CARTESIAN_POINT ( 'NONE',  ( -26.49999999999999289, -216.4061698243480976, 71.49757942303730829 ) ) ;
#5195 = CARTESIAN_POINT ( 'NONE',  ( 217.0000000000000000, -56.99999999999999289, 7.000000000000000000 ) ) ;
#5196 = EDGE_LOOP ( 'NONE', ( #7344, #5517, #1875, #2901 ) ) ;
#5197 = LINE ( 'NONE', #1039, #5915 ) ;
#5198 = DIRECTION ( 'NONE',  ( 1.000000000000000000, -5.551115123125783935E-17, 4.237045877651919561E-33 ) ) ;
#5199 = EDGE_CURVE ( 'NONE', #797, #1980, #3468, .T. ) ;
#5200 = EDGE_LOOP ( 'NONE', ( #5385, #3732, #806, #4257 ) ) ;
#5201 = CIRCLE ( 'NONE', #6021, 14.00000000000000533 ) ;
#5202 = CARTESIAN_POINT ( 'NONE',  ( 209.9999999999999716, 6.000000000000000000, 41.00000000000002132 ) ) ;
#5203 = CARTESIAN_POINT ( 'NONE',  ( 10.01709100512437267, -212.7665347604136343, 94.27567702562227225 ) ) ;
#5204 = ORIENTED_EDGE ( 'NONE', *, *, #2200, .T. ) ;
#5205 = ITEM_DEFINED_TRANSFORMATION ( 'NONE', 'NONE', #1534,  #1914 ) ;
#5206 = CARTESIAN_POINT ( 'NONE',  ( 3.000000000000000000, 56.99999999999999289, 3.000000000000021760 ) ) ;
#5207 = DIRECTION ( 'NONE',  ( 3.697785493223493385E-32, 0.7071067811865485719, 0.7071067811865464625 ) ) ;
#5208 =( REPRESENTATION_RELATIONSHIP ('NONE','NONE', #4862, #2538 ) REPRESENTATION_RELATIONSHIP_WITH_TRANSFORMATION ( #4936 )SHAPE_REPRESENTATION_RELATIONSHIP( ) );
#5209 = EDGE_CURVE ( 'NONE', #2155, #1164, #3378, .T. ) ;
#5210 = ORIENTED_EDGE ( 'NONE', *, *, #1141, .T. ) ;
#5211 = ORIENTED_EDGE ( 'NONE', *, *, #2405, .T. ) ;
#5212 = CYLINDRICAL_SURFACE ( 'NONE', #5252, 15.99999999999997335 ) ;
#5213 = AXIS2_PLACEMENT_3D ( 'NONE', #1930, #2504, #4280 ) ;
#5214 = CIRCLE ( 'NONE', #2628, 9.999999999999994671 ) ;
#5215 = DIRECTION ( 'NONE',  ( 0.000000000000000000, 0.000000000000000000, 1.000000000000000000 ) ) ;
#5216 = LINE ( 'NONE', #673, #1162 ) ;
#5217 = CARTESIAN_POINT ( 'NONE',  ( 2.775557561562891351E-14, 86.00000000000000000, 9.999999999999996447 ) ) ;
#5218 = CARTESIAN_POINT ( 'NONE',  ( 21.18129193964234958, -223.0630240738404950, 81.69876281950602959 ) ) ;
#5219 = CARTESIAN_POINT ( 'NONE',  ( 12.50000000000001066, 12.50000000000001066, -1.214306433183764966E-14 ) ) ;
#5220 = CARTESIAN_POINT ( 'NONE',  ( -61.32863543632851133, -218.0630603687720281, 75.59213739089364026 ) ) ;
#5221 = AXIS2_PLACEMENT_3D ( 'NONE', #3562, #5833, #7591 ) ;
#5222 = ADVANCED_FACE ( 'NONE', ( #6924 ), #5694, .T. ) ;
#5223 = AXIS2_PLACEMENT_3D ( 'NONE', #2732, #1498, #6817 ) ;
#5224 = EDGE_LOOP ( 'NONE', ( #6809, #1333, #1646, #6342 ) ) ;
#5225 = CARTESIAN_POINT ( 'NONE',  ( 1.387778780781445676E-14, 31.53553390593269512, 6.464466094067257806 ) ) ;
#5226 = FACE_OUTER_BOUND ( 'NONE', #1547, .T. ) ;
#5227 = CYLINDRICAL_SURFACE ( 'NONE', #6807, 10.00000000000000355 ) ;
#5228 = DIRECTION ( 'NONE',  ( 1.000000000000000000, 0.000000000000000000, 0.000000000000000000 ) ) ;
#5229 = AXIS2_PLACEMENT_3D ( 'NONE', #6850, #7426, #6188 ) ;
#5230 = VECTOR ( 'NONE', #4489, 1000.000000000000114 ) ;
#5231 = CARTESIAN_POINT ( 'NONE',  ( 21.50000000000000000, -223.0630240738404382, 73.28127814332047762 ) ) ;
#5232 = EDGE_CURVE ( 'NONE', #1421, #459, #3504, .T. ) ;
#5233 = ORIENTED_EDGE ( 'NONE', *, *, #3899, .F. ) ;
#5234 = AXIS2_PLACEMENT_3D ( 'NONE', #5052, #7390, #1616 ) ;
#5235 = VERTEX_POINT ( 'NONE', #7423 ) ;
#5236 = DIRECTION ( 'NONE',  ( -1.000000000000000000, 0.000000000000000000, -4.237045877651919561E-33 ) ) ;
#5237 = DIRECTION ( 'NONE',  ( 1.000000000000000000, 0.000000000000000000, 0.000000000000000000 ) ) ;
#5238 = ORIENTED_EDGE ( 'NONE', *, *, #4852, .T. ) ;
#5239 = DIRECTION ( 'NONE',  ( -1.000000000000000000, -0.000000000000000000, -0.000000000000000000 ) ) ;
#5240 = FACE_OUTER_BOUND ( 'NONE', #2566, .T. ) ;
#5241 = ORIENTED_EDGE ( 'NONE', *, *, #6910, .T. ) ;
#5242 = VECTOR ( 'NONE', #3661, 1000.000000000000000 ) ;
#5243 = EDGE_CURVE ( 'NONE', #5657, #2284, #1748, .T. ) ;
#5244 = DIRECTION ( 'NONE',  ( 1.000000000000000000, 2.465190328815661892E-32, -9.244463733058732095E-33 ) ) ;
#5245 = CARTESIAN_POINT ( 'NONE',  ( 17.66255603274094454, -212.1022451272886542, 94.15854484029739524 ) ) ;
#5246 = EDGE_LOOP ( 'NONE', ( #6045, #2472, #4128, #7016 ) ) ;
#5247 = APPLICATION_PROTOCOL_DEFINITION ( 'draft international standard', 'automotive_design', 1998, #2693 ) ;
#5248 = CARTESIAN_POINT ( 'NONE',  ( 43.50000000000001421, 39.99999999999999289, 0.000000000000000000 ) ) ;
#5249 = CARTESIAN_POINT ( 'NONE',  ( 47.00000000000000000, 30.03170604878415162, 13.00000000000001066 ) ) ;
#5250 = AXIS2_PLACEMENT_3D ( 'NONE', #4913, #4487, #4333 ) ;
#5251 = EDGE_LOOP ( 'NONE', ( #5854, #6510, #3235, #2321 ) ) ;
#5252 = AXIS2_PLACEMENT_3D ( 'NONE', #7478, #1623, #7515 ) ;
#5253 = DIRECTION ( 'NONE',  ( -1.000000000000000000, -0.000000000000000000, -0.000000000000000000 ) ) ;
#5254 = CARTESIAN_POINT ( 'NONE',  ( 0.000000000000000000, 0.000000000000000000, -39.99999999999997868 ) ) ;
#5255 = CARTESIAN_POINT ( 'NONE',  ( 0.000000000000000000, 35.07106781186547551, 2.928932188134525827 ) ) ;
#5256 = CARTESIAN_POINT ( 'NONE',  ( 18.38715965971085353, -218.0630240738404950, 75.65381970816498836 ) ) ;
#5257 = CARTESIAN_POINT ( 'NONE',  ( -21.50000000000000000, -114.3401965514817960, 42.31370849898471675 ) ) ;
#5258 = B_SPLINE_CURVE_WITH_KNOTS ( 'NONE', 3,
 ( #5000, #294, #6137, #7367, #3802, #979, #1446, #2640, #1477, #2100 ),
 .UNSPECIFIED., .F., .F.,
 ( 4, 2, 2, 2, 4 ),
 ( -1.095445419986480569E-05, 0.001102508244345350684, 0.002215970942890566238, 0.003329433641435781792, 0.004442896339980997346 ),
 .UNSPECIFIED. ) ;
#5259 = CARTESIAN_POINT ( 'NONE',  ( 170.0000000000000000, -11.00000000000000355, 8.660254037844387298 ) ) ;
#5260 = PRODUCT_DEFINITION_CONTEXT ( 'detailed design', #3890, 'design' ) ;
#5261 = ORIENTED_EDGE ( 'NONE', *, *, #4249, .T. ) ;
#5262 = EDGE_LOOP ( 'NONE', ( #1767, #250, #7287, #844 ) ) ;
#5263 = EDGE_CURVE ( 'NONE', #6977, #5737, #1033, .T. ) ;
#5264 = CARTESIAN_POINT ( 'NONE',  ( -64.50000000000000000, -223.0630240738404950, 73.28127814332044920 ) ) ;
#5265 = CARTESIAN_POINT ( 'NONE',  ( 217.0000000000000000, 15.00000000000000000, 15.00000000000000888 ) ) ;
#5266 = LINE ( 'NONE', #2451, #2525 ) ;
#5267 = DIRECTION ( 'NONE',  ( -2.465190328815661892E-32, -1.000000000000000000, -1.193489751472043281E-15 ) ) ;
#5268 = EDGE_CURVE ( 'NONE', #1421, #1604, #3966, .T. ) ;
#5269 = CARTESIAN_POINT ( 'NONE',  ( 188.2950735375078750, -5.838146261106893498, 17.40596459241342231 ) ) ;
#5270 = VERTEX_POINT ( 'NONE', #1651 ) ;
#5271 = ORIENTED_EDGE ( 'NONE', *, *, #6333, .T. ) ;
#5272 = CYLINDRICAL_SURFACE ( 'NONE', #6361, 26.99999999999999289 ) ;
#5273 = FACE_BOUND ( 'NONE', #2886, .T. ) ;
#5274 = EDGE_CURVE ( 'NONE', #5684, #3448, #4008, .T. ) ;
#5275 = ORIENTED_EDGE ( 'NONE', *, *, #4421, .T. ) ;
#5276 = DIRECTION ( 'NONE',  ( -8.747574602982985342E-17, -0.9659258262890683122, 0.2588190451025207950 ) ) ;
#5277 = FACE_OUTER_BOUND ( 'NONE', #4662, .T. ) ;
#5278 = VERTEX_POINT ( 'NONE', #3927 ) ;
#5279 = EDGE_LOOP ( 'NONE', ( #1611, #6230, #1848, #4372 ) ) ;
#5280 = DIRECTION ( 'NONE',  ( 0.000000000000000000, 0.000000000000000000, 1.000000000000000000 ) ) ;
#5281 = CARTESIAN_POINT ( 'NONE',  ( 53.00000000000000711, -20.99999999999999645, 10.00000000000000888 ) ) ;
#5282 = ORIENTED_EDGE ( 'NONE', *, *, #5531, .T. ) ;
#5283 = PRODUCT_CONTEXT ( 'NONE', #1270, 'mechanical' ) ;
#5284 = DIRECTION ( 'NONE',  ( -1.000000000000000000, 1.294224922628222493E-31, -1.078147950931789264E-16 ) ) ;
#5285 = VERTEX_POINT ( 'NONE', #5740 ) ;
#5286 = DIRECTION ( 'NONE',  ( -0.8660254037844413721, 0.000000000000000000, 0.4999999999999950595 ) ) ;
#5287 = CIRCLE ( 'NONE', #1467, 10.00000000000000711 ) ;
#5288 = PLANE ( 'NONE',  #3131 ) ;
#5289 =( NAMED_UNIT ( * ) PLANE_ANGLE_UNIT ( ) SI_UNIT ( $, .RADIAN. ) );
#5290 = CARTESIAN_POINT ( 'NONE',  ( 18.25938667636025059, -218.0630240738405234, 75.51685001270919884 ) ) ;
#5291 = CARTESIAN_POINT ( 'NONE',  ( 20.45699128574564085, -223.0630240738404666, 89.66439215578999722 ) ) ;
#5292 = DIRECTION ( 'NONE',  ( -0.000000000000000000, 1.000000000000000000, 2.065146995210484941E-16 ) ) ;
#5293 = PRODUCT ( 'right arm', 'right arm', '', ( #5863 ) ) ;
#5294 = EDGE_CURVE ( 'NONE', #2976, #2821, #7427, .T. ) ;
#5295 = AXIS2_PLACEMENT_3D ( 'NONE', #2819, #2206, #5170 ) ;
#5296 = ORIENTED_EDGE ( 'NONE', *, *, #6500, .F. ) ;
#5297 = CARTESIAN_POINT ( 'NONE',  ( 209.9999999999999716, -6.000000000000000000, 18.00000000000001066 ) ) ;
#5298 = CARTESIAN_POINT ( 'NONE',  ( 220.0000000000000000, 9.000000000000001776, 18.00000000000001066 ) ) ;
#5299 = CARTESIAN_POINT ( 'NONE',  ( 187.2209186502361149, 6.851382254476026112, 15.00000000000001066 ) ) ;
#5300 = CIRCLE ( 'NONE', #4937, 25.00000000000000000 ) ;
#5301 = DIRECTION ( 'NONE',  ( 5.551115123125783935E-17, 1.000000000000000000, 5.166928274020107347E-17 ) ) ;
#5302 = EDGE_CURVE ( 'NONE', #3744, #6935, #3129, .T. ) ;
#5303 = VERTEX_POINT ( 'NONE', #6390 ) ;
#5304 = ORIENTED_EDGE ( 'NONE', *, *, #7262, .T. ) ;
#5305 = CARTESIAN_POINT ( 'NONE',  ( 0.000000000000000000, 0.000000000000000000, -9.999999999999994671 ) ) ;
#5306 = CIRCLE ( 'NONE', #6656, 17.99999999999999645 ) ;
#5307 = CYLINDRICAL_SURFACE ( 'NONE', #1897, 6.000000000000000000 ) ;
#5308 = ORIENTED_EDGE ( 'NONE', *, *, #6363, .T. ) ;
#5309 = CARTESIAN_POINT ( 'NONE',  ( -53.00237955168407922, -217.4114710059382674, 71.76694906279446684 ) ) ;
#5310 = CARTESIAN_POINT ( 'NONE',  ( 48.51085693943327470, -25.40781859939735199, 12.90851588443849174 ) ) ;
#5311 = CARTESIAN_POINT ( 'NONE',  ( 25.00000000000000000, 31.53553390593274841, 6.464466094067261359 ) ) ;
#5312 = VERTEX_POINT ( 'NONE', #532 ) ;
#5313 = AXIS2_PLACEMENT_3D ( 'NONE', #7227, #4310, #7342 ) ;
#5314 = EDGE_CURVE ( 'NONE', #2069, #4378, #6884, .T. ) ;
#5315 = ORIENTED_EDGE ( 'NONE', *, *, #152, .T. ) ;
#5316 = DIRECTION ( 'NONE',  ( -5.605193857299270773E-45, -0.000000000000000000, -1.000000000000000000 ) ) ;
#5317 = CARTESIAN_POINT ( 'NONE',  ( 17.72636667137882682, -216.4242598635584613, 94.92063264932014022 ) ) ;
#5318 = VERTEX_POINT ( 'NONE', #7574 ) ;
#5319 = APPLICATION_PROTOCOL_DEFINITION ( 'draft international standard', 'automotive_design', 1998, #1916 ) ;
#5320 = CARTESIAN_POINT ( 'NONE',  ( -30.49999999999998579, -214.0630240738404666, 96.09122589815579829 ) ) ;
#5321 = DIRECTION ( 'NONE',  ( 0.000000000000000000, -3.304235192336777977E-16, 1.000000000000000000 ) ) ;
#5322 = VERTEX_POINT ( 'NONE', #997 ) ;
#5323 = EDGE_CURVE ( 'NONE', #6005, #1310, #422, .T. ) ;
#5324 = FACE_BOUND ( 'NONE', #622, .T. ) ;
#5325 = DIRECTION ( 'NONE',  ( 1.000000000000000000, 0.000000000000000000, 0.000000000000000000 ) ) ;
#5326 = ORIENTED_EDGE ( 'NONE', *, *, #6654, .T. ) ;
#5327 = CARTESIAN_POINT ( 'NONE',  ( 21.28788537653265323, -218.0630240738404666, 86.14873225104479104 ) ) ;
#5328 = AXIS2_PLACEMENT_3D ( 'NONE', #1404, #4918, #3689 ) ;
#5329 = DIRECTION ( 'NONE',  ( 0.000000000000000000, 0.000000000000000000, -1.000000000000000000 ) ) ;
#5330 = DIRECTION ( 'NONE',  ( -1.000000000000000000, -0.000000000000000000, -0.000000000000000000 ) ) ;
#5331 = PRODUCT_DEFINITION_SHAPE ( 'NONE', 'NONE',  #7606 ) ;
#5332 = UNCERTAINTY_MEASURE_WITH_UNIT (LENGTH_MEASURE( 1.000000000000000082E-05 ), #6857, 'distance_accuracy_value', 'NONE');
#5333 = ORIENTED_EDGE ( 'NONE', *, *, #5809, .T. ) ;
#5334 = AXIS2_PLACEMENT_3D ( 'NONE', #6769, #7272, #311 ) ;
#5335 =( GEOMETRIC_REPRESENTATION_CONTEXT ( 3 ) GLOBAL_UNCERTAINTY_ASSIGNED_CONTEXT ( ( #7025 ) ) GLOBAL_UNIT_ASSIGNED_CONTEXT ( ( #3799, #715, #1362 ) ) REPRESENTATION_CONTEXT ( 'NONE', 'WORKASPACE' ) );
#5336 = ORIENTED_EDGE ( 'NONE', *, *, #3100, .T. ) ;
#5337 = CARTESIAN_POINT ( 'NONE',  ( 0.000000000000000000, 27.04312195450891565, 12.73853277175702559 ) ) ;
#5338 = DIRECTION ( 'NONE',  ( -1.681558157189779738E-44, 0.000000000000000000, -1.000000000000000000 ) ) ;
#5339 = CARTESIAN_POINT ( 'NONE',  ( 3.000000000000002665, -22.89008536370703695, 9.895301509892497904 ) ) ;
#5340 = CARTESIAN_POINT ( 'NONE',  ( -13.35769912250762914, -65.39789427971170710, 38.39789427971182789 ) ) ;
#5341 = ADVANCED_FACE ( 'NONE', ( #5774 ), #5122, .T. ) ;
#5342 = CARTESIAN_POINT ( 'NONE',  ( 217.0000000000000000, 15.08392021690038121, 12.00000000000000711 ) ) ;
#5343 = DIRECTION ( 'NONE',  ( 0.000000000000000000, 0.000000000000000000, -1.000000000000000000 ) ) ;
#5344 = AXIS2_PLACEMENT_3D ( 'NONE', #5195, #3435, #5656 ) ;
#5345 = PRESENTATION_LAYER_ASSIGNMENT (  '', '', ( #6566 ) ) ;
#5346 = VECTOR ( 'NONE', #5189, 1000.000000000000000 ) ;
#5347 = ORIENTED_EDGE ( 'NONE', *, *, #3338, .T. ) ;
#5348 = ORIENTED_EDGE ( 'NONE', *, *, #2725, .F. ) ;
#5349 = VECTOR ( 'NONE', #2875, 1000.000000000000000 ) ;
#5350 = AXIS2_PLACEMENT_3D ( 'NONE', #2404, #514, #5215 ) ;
#5351 = CIRCLE ( 'NONE', #796, 2.999999999999999112 ) ;
#5352 = CARTESIAN_POINT ( 'NONE',  ( -26.50000000000000711, -125.0933926253236450, 30.46597562735434295 ) ) ;
#5353 =( BOUNDED_CURVE ( )  B_SPLINE_CURVE ( 3, ( #763, #1266, #159, #2348 ),
 .UNSPECIFIED., .F., .T. ) 
 B_SPLINE_CURVE_WITH_KNOTS ( ( 4, 4 ),
 ( 4.712388980384686121, 5.585053606381841895 ),
 .UNSPECIFIED. ) 
 CURVE ( )  GEOMETRIC_REPRESENTATION_ITEM ( )  RATIONAL_B_SPLINE_CURVE ( ( 1.000000000000000000, 0.9375385246911012160, 0.9375385246911012160, 1.000000000000000000 ) ) 
 REPRESENTATION_ITEM ( '' )  );
#5354 = CARTESIAN_POINT ( 'NONE',  ( 21.50000000000000000, -49.37258300203045280, -2.775557561562891351E-14 ) ) ;
#5355 = VERTEX_POINT ( 'NONE', #7533 ) ;
#5356 = CARTESIAN_POINT ( 'NONE',  ( -60.68960140267981274, -218.8824061789508733, 72.16108495452549221 ) ) ;
#5357 = LINE ( 'NONE', #86, #502 ) ;
#5358 = CARTESIAN_POINT ( 'NONE',  ( 26.49999999999999645, -39.99999999999999289, 0.000000000000000000 ) ) ;
#5359 = VERTEX_POINT ( 'NONE', #2846 ) ;
#5360 = ORIENTED_EDGE ( 'NONE', *, *, #363, .F. ) ;
#5361 = FACE_OUTER_BOUND ( 'NONE', #2847, .T. ) ;
#5362 = CARTESIAN_POINT ( 'NONE',  ( -26.50000000000003197, 0.000000000000000000, 0.000000000000000000 ) ) ;
#5363 = VERTEX_POINT ( 'NONE', #2278 ) ;
#5364 = DIRECTION ( 'NONE',  ( 1.000000000000000000, 0.000000000000000000, 0.000000000000000000 ) ) ;
#5365 = ADVANCED_FACE ( 'NONE', ( #461 ), #2808, .T. ) ;
#5366 = CARTESIAN_POINT ( 'NONE',  ( 220.0000000000000000, 3.000000000000000000, 35.00000000000000000 ) ) ;
#5367 = CARTESIAN_POINT ( 'NONE',  ( -64.50000000000000000, -60.68629150101525482, -11.31370849898474873 ) ) ;
#5368 = ORIENTED_EDGE ( 'NONE', *, *, #2252, .F. ) ;
#5369 = AXIS2_PLACEMENT_3D ( 'NONE', #194, #834, #1953 ) ;
#5370 = CARTESIAN_POINT ( 'NONE',  ( 0.000000000000000000, 0.000000000000000000, -39.99999999999997868 ) ) ;
#5371 = CARTESIAN_POINT ( 'NONE',  ( 3.000000000000002665, -60.00000000000000000, 3.000000000000000444 ) ) ;
#5372 = VERTEX_POINT ( 'NONE', #6967 ) ;
#5373 = DIRECTION ( 'NONE',  ( 0.000000000000000000, -2.065146995210484448E-16, 1.000000000000000000 ) ) ;
#5374 = EDGE_CURVE ( 'NONE', #5934, #570, #7544, .T. ) ;
#5375 = DIRECTION ( 'NONE',  ( 9.231085635203014490E-31, 0.000000000000000000, -1.000000000000000000 ) ) ;
#5376 = DIRECTION ( 'NONE',  ( -0.000000000000000000, 1.000000000000000000, -0.000000000000000000 ) ) ;
#5377 = ADVANCED_FACE ( 'NONE', ( #649 ), #5923, .T. ) ;
#5378 = CARTESIAN_POINT ( 'NONE',  ( 217.0000000000000000, 0.000000000000000000, 12.00000000000000711 ) ) ;
#5379 = CARTESIAN_POINT ( 'NONE',  ( -29.50000000000000000, -215.0630240738404950, 73.28127814332047762 ) ) ;
#5380 = DIRECTION ( 'NONE',  ( 5.605193857299270773E-45, 0.000000000000000000, 1.000000000000000000 ) ) ;
#5381 = DIRECTION ( 'NONE',  ( -1.000000000000000000, 0.000000000000000000, 0.000000000000000000 ) ) ;
#5382 = CARTESIAN_POINT ( 'NONE',  ( -32.50000000000002842, -60.68629150101524772, -11.31370849898474873 ) ) ;
#5383 = CARTESIAN_POINT ( 'NONE',  ( 25.00000000000000000, 31.53553390593274841, 6.464466094067261359 ) ) ;
#5384 = AXIS2_PLACEMENT_3D ( 'NONE', #1185, #1111, #5236 ) ;
#5385 = ORIENTED_EDGE ( 'NONE', *, *, #2252, .T. ) ;
#5386 = ADVANCED_FACE ( 'NONE', ( #4746 ), #5307, .F. ) ;
#5387 = ORIENTED_EDGE ( 'NONE', *, *, #1352, .T. ) ;
#5388 = CARTESIAN_POINT ( 'NONE',  ( 25.00000000000002132, 73.78679656440357348, 0.9999999999999991118 ) ) ;
#5389 = CARTESIAN_POINT ( 'NONE',  ( -53.25365409304692577, -218.1074892565141283, 95.21743140602096389 ) ) ;
#5390 = ORIENTED_EDGE ( 'NONE', *, *, #1977, .F. ) ;
#5391 = CARTESIAN_POINT ( 'NONE',  ( -70.24145449743711822, -214.0092129552773201, 88.67031792470811524 ) ) ;
#5392 = PLANE ( 'NONE',  #3824 ) ;
#5393 = CARTESIAN_POINT ( 'NONE',  ( -57.20103464615607436, -218.0628873493838000, 94.48139145718995735 ) ) ;
#5394 = VERTEX_POINT ( 'NONE', #2346 ) ;
#5395 = EDGE_CURVE ( 'NONE', #6501, #5696, #6189, .T. ) ;
#5396 = ORIENTED_EDGE ( 'NONE', *, *, #5864, .T. ) ;
#5397 =( BOUNDED_CURVE ( )  B_SPLINE_CURVE ( 3, ( #5698, #425, #5125, #7467 ),
 .UNSPECIFIED., .F., .T. ) 
 B_SPLINE_CURVE_WITH_KNOTS ( ( 4, 4 ),
 ( 4.712388980384690562, 6.115737227959895606 ),
 .UNSPECIFIED. ) 
 CURVE ( )  GEOMETRIC_REPRESENTATION_ITEM ( )  RATIONAL_B_SPLINE_CURVE ( ( 1.000000000000000000, 0.8425084105506492893, 0.8425084105506492893, 1.000000000000000000 ) ) 
 REPRESENTATION_ITEM ( '' )  );
#5398 = DIRECTION ( 'NONE',  ( -5.605193857299269528E-45, 0.000000000000000000, 1.000000000000000000 ) ) ;
#5399 = CARTESIAN_POINT ( 'NONE',  ( 17.83909347413333890, -228.8136496942591975, 74.82215363428539945 ) ) ;
#5400 = EDGE_LOOP ( 'NONE', ( #1943, #7122 ) ) ;
#5401 = DIRECTION ( 'NONE',  ( 1.000000000000000000, 2.624548829666596736E-30, -9.231085635203017994E-31 ) ) ;
#5402 = CYLINDRICAL_SURFACE ( 'NONE', #6087, 6.000000000000015987 ) ;
#5403 = ORIENTED_EDGE ( 'NONE', *, *, #5199, .F. ) ;
#5404 = ADVANCED_FACE ( 'NONE', ( #724 ), #1921, .T. ) ;
#5405 = PLANE ( 'NONE',  #5989 ) ;
#5406 = DIRECTION ( 'NONE',  ( 1.000000000000000000, 0.000000000000000000, 0.000000000000000000 ) ) ;
#5407 = DIRECTION ( 'NONE',  ( 0.000000000000000000, 0.000000000000000000, 1.000000000000000000 ) ) ;
#5408 = CARTESIAN_POINT ( 'NONE',  ( -32.50000000000002842, 16.00000000000012079, -15.99999999999995914 ) ) ;
#5409 = PRESENTATION_LAYER_ASSIGNMENT (  '', '', ( #3568 ) ) ;
#5410 = CARTESIAN_POINT ( 'NONE',  ( 25.00000000000000000, 40.21320343559644783, 5.999999999999996447 ) ) ;
#5411 = UNCERTAINTY_MEASURE_WITH_UNIT (LENGTH_MEASURE( 1.000000000000000082E-05 ), #1055, 'distance_accuracy_value', 'NONE');
#5412 = VECTOR ( 'NONE', #6527, 1000.000000000000000 ) ;
#5413 = EDGE_CURVE ( 'NONE', #4312, #4326, #4273, .T. ) ;
#5414 = EDGE_CURVE ( 'NONE', #7581, #2056, #2921, .T. ) ;
#5415 = CIRCLE ( 'NONE', #4683, 9.999999999999998224 ) ;
#5416 = CYLINDRICAL_SURFACE ( 'NONE', #3411, 8.000000000000007105 ) ;
#5417 = CARTESIAN_POINT ( 'NONE',  ( -16.50000000000000355, -99.90626354475340065, 72.90626354475362803 ) ) ;
#5418 = DIRECTION ( 'NONE',  ( 0.000000000000000000, 0.000000000000000000, 1.000000000000000000 ) ) ;
#5419 = CARTESIAN_POINT ( 'NONE',  ( 191.2361162513372221, -6.000000000000000000, 16.49999999999999289 ) ) ;
#5420 = DIRECTION ( 'NONE',  ( -1.000000000000000000, -0.000000000000000000, -0.000000000000000000 ) ) ;
#5421 = CARTESIAN_POINT ( 'NONE',  ( 189.5040654437683258, -3.000000000000000888, 19.50000000000000355 ) ) ;
#5422 = AXIS2_PLACEMENT_3D ( 'NONE', #6163, #6784, #6710 ) ;
#5423 = EDGE_LOOP ( 'NONE', ( #936, #3967, #5497, #4150 ) ) ;
#5424 = EDGE_CURVE ( 'NONE', #5460, #1413, #6788, .T. ) ;
#5425 = ORIENTED_EDGE ( 'NONE', *, *, #5294, .T. ) ;
#5426 = LINE ( 'NONE', #263, #6595 ) ;
#5427 = DIRECTION ( 'NONE',  ( 0.000000000000000000, 0.000000000000000000, 1.000000000000000000 ) ) ;
#5428 = CARTESIAN_POINT ( 'NONE',  ( -70.12317295347672541, -221.7587214059827261, 78.74778750054862542 ) ) ;
#5429 = FILL_AREA_STYLE_COLOUR ( '', #5183 ) ;
#5430 = CARTESIAN_POINT ( 'NONE',  ( -56.75063899659176059, -218.0625894763260817, 94.64364256205048775 ) ) ;
#5431 = B_SPLINE_CURVE_WITH_KNOTS ( 'NONE', 3,
 ( #2788, #6445, #1054, #2823 ),
 .UNSPECIFIED., .F., .F.,
 ( 4, 4 ),
 ( 0.000000000000000000, 0.0005182278649586876925 ),
 .UNSPECIFIED. ) ;
#5432 = ORIENTED_EDGE ( 'NONE', *, *, #2775, .T. ) ;
#5433 = ORIENTED_EDGE ( 'NONE', *, *, #7238, .T. ) ;
#5434 = VECTOR ( 'NONE', #6056, 1000.000000000000000 ) ;
#5435 = CARTESIAN_POINT ( 'NONE',  ( 3.000000000000002665, -18.00000000000000000, 10.00000000000000888 ) ) ;
#5436 = CARTESIAN_POINT ( 'NONE',  ( 25.00000000000002842, 73.78679656440351664, 11.00000000000000178 ) ) ;
#5437 = VERTEX_POINT ( 'NONE', #1263 ) ;
#5438 = EDGE_CURVE ( 'NONE', #2174, #5858, #6321, .T. ) ;
#5439 = PLANE ( 'NONE',  #3463 ) ;
#5440 = FACE_BOUND ( 'NONE', #5979, .T. ) ;
#5441 = VECTOR ( 'NONE', #1418, 1000.000000000000000 ) ;
#5442 = ORIENTED_EDGE ( 'NONE', *, *, #242, .F. ) ;
#5443 = DIRECTION ( 'NONE',  ( 0.000000000000000000, 0.000000000000000000, 1.000000000000000000 ) ) ;
#5444 = DIRECTION ( 'NONE',  ( -1.000000000000000000, 0.000000000000000000, -7.663350976776343357E-46 ) ) ;
#5445 = VERTEX_POINT ( 'NONE', #5885 ) ;
#5446 =( LENGTH_UNIT ( ) NAMED_UNIT ( * ) SI_UNIT ( .MILLI., .METRE. ) );
#5447 = ADVANCED_FACE ( 'NONE', ( #5273, #5963 ), #157, .T. ) ;
#5448 = DIRECTION ( 'NONE',  ( -1.000000000000000000, 0.000000000000000000, 0.000000000000000000 ) ) ;
#5449 = CARTESIAN_POINT ( 'NONE',  ( 188.0000000000000000, -14.00000000000000711, 0.000000000000000000 ) ) ;
#5450 = CARTESIAN_POINT ( 'NONE',  ( 0.000000000000000000, 0.000000000000000000, -9.999999999999994671 ) ) ;
#5451 = ORIENTED_EDGE ( 'NONE', *, *, #1566, .T. ) ;
#5452 = DIRECTION ( 'NONE',  ( 1.000000000000000000, 0.000000000000000000, 5.605193857299269528E-45 ) ) ;
#5453 = CARTESIAN_POINT ( 'NONE',  ( 185.0000000000000000, 39.99999999999999289, 10.00000000000000355 ) ) ;
#5454 = CARTESIAN_POINT ( 'NONE',  ( -21.48215622306531003, -113.7796841263388501, 41.77968412633906325 ) ) ;
#5455 = CARTESIAN_POINT ( 'NONE',  ( -64.34084354375256964, -223.0645981545465588, 82.82631477277033127 ) ) ;
#5456 = CARTESIAN_POINT ( 'NONE',  ( -13.49999999999999822, -223.0630240738404382, 73.28127814332047762 ) ) ;
#5457 = EDGE_CURVE ( 'NONE', #7358, #3833, #2633, .T. ) ;
#5458 = CIRCLE ( 'NONE', #2130, 5.000000000000004441 ) ;
#5459 = AXIS2_PLACEMENT_3D ( 'NONE', #3419, #2257, #5758 ) ;
#5460 = VERTEX_POINT ( 'NONE', #7192 ) ;
#5461 = EDGE_LOOP ( 'NONE', ( #6578, #5644 ) ) ;
#5462 = CARTESIAN_POINT ( 'NONE',  ( 217.0000000000000000, -20.99999999999999645, 13.00000000000000888 ) ) ;
#5463 = AXIS2_PLACEMENT_3D ( 'NONE', #5747, #5820, #467 ) ;
#5464 = CARTESIAN_POINT ( 'NONE',  ( 30.00000000000000000, 1.102182119232615150E-15, -8.000000000000000000 ) ) ;
#5465 = VECTOR ( 'NONE', #5566, 1000.000000000000000 ) ;
#5466 = AXIS2_PLACEMENT_3D ( 'NONE', #6054, #3790, #850 ) ;
#5467 = CARTESIAN_POINT ( 'NONE',  ( -53.50256896896199521, -228.4878731603045026, 74.73486207509921542 ) ) ;
#5468 = DIRECTION ( 'NONE',  ( -9.244463733058732095E-33, -4.557872517964703399E-64, -1.000000000000000000 ) ) ;
#5469 = EDGE_CURVE ( 'NONE', #2726, #3811, #3628, .T. ) ;
#5470 = CARTESIAN_POINT ( 'NONE',  ( -58.28420576404219133, -218.0630240738404382, 94.02398971667126659 ) ) ;
#5471 = VERTEX_POINT ( 'NONE', #3507 ) ;
#5472 = AXIS2_PLACEMENT_3D ( 'NONE', #6847, #2156, #3396 ) ;
#5473 = VECTOR ( 'NONE', #977, 1000.000000000000000 ) ;
#5474 = ORIENTED_EDGE ( 'NONE', *, *, #4043, .F. ) ;
#5475 = CARTESIAN_POINT ( 'NONE',  ( -16.49999999999996447, -99.90626354475340065, 72.90626354475362803 ) ) ;
#5476 = CARTESIAN_POINT ( 'NONE',  ( 24.99999999999998579, 101.4999999999999858, 9.999999999999996447 ) ) ;
#5477 = ORIENTED_EDGE ( 'NONE', *, *, #4471, .F. ) ;
#5478 = CIRCLE ( 'NONE', #5229, 14.00000000000000533 ) ;
#5479 = CARTESIAN_POINT ( 'NONE',  ( 209.9999999999999716, 6.000000000000000000, 35.00000000000000000 ) ) ;
#5480 = DIRECTION ( 'NONE',  ( 0.000000000000000000, 0.000000000000000000, -1.000000000000000000 ) ) ;
#5481 = ORIENTED_EDGE ( 'NONE', *, *, #7525, .T. ) ;
#5482 = EDGE_CURVE ( 'NONE', #1226, #3851, #4163, .T. ) ;
#5483 = ADVANCED_FACE ( 'NONE', ( #7038 ), #1765, .F. ) ;
#5484 = CARTESIAN_POINT ( 'NONE',  ( -18.18629150101523351, -223.0630240738404382, 73.28127814332044920 ) ) ;
#5485 = LINE ( 'NONE', #708, #3009 ) ;
#5486 = DIRECTION ( 'NONE',  ( 0.000000000000000000, 0.000000000000000000, 1.000000000000000000 ) ) ;
#5487 = DIRECTION ( 'NONE',  ( -1.000000000000000000, 0.000000000000000000, 0.000000000000000000 ) ) ;
#5488 = PLANE ( 'NONE',  #6392 ) ;
#5489 = EDGE_LOOP ( 'NONE', ( #4638, #6980, #5137, #3623 ) ) ;
#5490 = DIRECTION ( 'NONE',  ( 1.681558157189779489E-44, -0.02411877311568872903, 0.9997091000803153271 ) ) ;
#5491 = DIRECTION ( 'NONE',  ( -1.000000000000000000, 5.551115123125783935E-17, -4.237045877651919561E-33 ) ) ;
#5492 = CARTESIAN_POINT ( 'NONE',  ( -24.50000000000000000, 16.00000000000006395, 30.68629150101531877 ) ) ;
#5493 = FACE_BOUND ( 'NONE', #6525, .T. ) ;
#5494 = CARTESIAN_POINT ( 'NONE',  ( -64.08458520774711076, -223.0616687716003241, 87.89351621351769950 ) ) ;
#5495 = DIRECTION ( 'NONE',  ( -3.379803290564628095E-16, -1.221245327087672392E-15, 1.000000000000000000 ) ) ;
#5496 = AXIS2_PLACEMENT_3D ( 'NONE', #252, #5175, #7590 ) ;
#5497 = ORIENTED_EDGE ( 'NONE', *, *, #591, .T. ) ;
#5498 = EDGE_CURVE ( 'NONE', #1269, #79, #1224, .T. ) ;
#5499 = ORIENTED_EDGE ( 'NONE', *, *, #756, .F. ) ;
#5500 = ADVANCED_FACE ( 'NONE', ( #6689 ), #6729, .F. ) ;
#5501 = DIRECTION ( 'NONE',  ( -1.000000000000000000, -1.853902270198408060E-44, -1.681558157189780485E-44 ) ) ;
#5502 = VECTOR ( 'NONE', #2085, 1000.000000000000000 ) ;
#5503 = CARTESIAN_POINT ( 'NONE',  ( -23.84314575050760965, -108.6568542494922127, 36.65685424949233351 ) ) ;
#5504 = CARTESIAN_POINT ( 'NONE',  ( -16.50000000000000355, -214.0630240738404382, 71.94153218116485959 ) ) ;
#5505 = PLANE ( 'NONE',  #4268 ) ;
#5506 = CARTESIAN_POINT ( 'NONE',  ( -64.49232742940240826, -218.0627193185516433, 84.13172309758257938 ) ) ;
#5507 = ORIENTED_EDGE ( 'NONE', *, *, #5605, .T. ) ;
#5508 = ORIENTED_EDGE ( 'NONE', *, *, #5004, .T. ) ;
#5509 = EDGE_CURVE ( 'NONE', #2575, #238, #2107, .T. ) ;
#5510 = ADVANCED_FACE ( 'NONE', ( #230 ), #3749, .T. ) ;
#5511 = CARTESIAN_POINT ( 'NONE',  ( -16.50000000000000000, -216.4061698243480976, 71.49757942303727987 ) ) ;
#5512 = CARTESIAN_POINT ( 'NONE',  ( 17.73846410710429211, -222.1285142276679210, 73.03087698472572242 ) ) ;
#5513 = VERTEX_POINT ( 'NONE', #3186 ) ;
#5514 = PRODUCT_RELATED_PRODUCT_CATEGORY ( 'part', '', ( #2227 ) ) ;
#5515 = LINE ( 'NONE', #239, #2838 ) ;
#5516 = CARTESIAN_POINT ( 'NONE',  ( -31.48397095257175238, -108.8525495989622414, 36.85254959896238347 ) ) ;
#5517 = ORIENTED_EDGE ( 'NONE', *, *, #5931, .T. ) ;
#5518 = FACE_OUTER_BOUND ( 'NONE', #4303, .T. ) ;
#5519 = CARTESIAN_POINT ( 'NONE',  ( 203.9378221735088630, 6.000000000000000000, 38.50000000000000000 ) ) ;
#5520 = ORIENTED_EDGE ( 'NONE', *, *, #6146, .F. ) ;
#5521 = CARTESIAN_POINT ( 'NONE',  ( 217.0000000000000000, -56.99999999999999289, 3.000000000000000444 ) ) ;
#5522 = CYLINDRICAL_SURFACE ( 'NONE', #5422, 8.500000000000007105 ) ;
#5523 = CARTESIAN_POINT ( 'NONE',  ( 3.000000000000002665, -25.88825784476432545, 10.00000000000001066 ) ) ;
#5524 = ORIENTED_EDGE ( 'NONE', *, *, #4001, .F. ) ;
#5525 = CARTESIAN_POINT ( 'NONE',  ( -64.50000000000000000, -223.0630240738404950, 96.09122589815579829 ) ) ;
#5526 = SURFACE_STYLE_USAGE ( .BOTH. , #1401 ) ;
#5527 = DIRECTION ( 'NONE',  ( -1.000000000000000000, 4.067564042545842122E-31, -3.379803290564627601E-16 ) ) ;
#5528 = CARTESIAN_POINT ( 'NONE',  ( -63.90555473623476956, -223.0625582585724942, 88.46971898607593232 ) ) ;
#5529 = ORIENTED_EDGE ( 'NONE', *, *, #5302, .T. ) ;
#5530 = CYLINDRICAL_SURFACE ( 'NONE', #2702, 4.000000000000003553 ) ;
#5531 = EDGE_CURVE ( 'NONE', #2238, #2601, #6812, .T. ) ;
#5532 = AXIS2_PLACEMENT_3D ( 'NONE', #5450, #5561, #3831 ) ;
#5533 = ORIENTED_EDGE ( 'NONE', *, *, #5126, .T. ) ;
#5534 = VERTEX_POINT ( 'NONE', #872 ) ;
#5535 = CARTESIAN_POINT ( 'NONE',  ( 47.00000000000000000, -28.78532416918554304, 10.00000000000000711 ) ) ;
#5536 = CARTESIAN_POINT ( 'NONE',  ( 217.0000000000000000, -18.00000000000000000, 10.00000000000000888 ) ) ;
#5537 = AXIS2_PLACEMENT_3D ( 'NONE', #4640, #3978, #7586 ) ;
#5538 = CYLINDRICAL_SURFACE ( 'NONE', #4947, 6.000000000000001776 ) ;
#5539 = EDGE_CURVE ( 'NONE', #1529, #7476, #4890, .T. ) ;
#5540 = FACE_OUTER_BOUND ( 'NONE', #813, .T. ) ;
#5541 = ORIENTED_EDGE ( 'NONE', *, *, #6731, .F. ) ;
#5542 = AXIS2_PLACEMENT_3D ( 'NONE', #5787, #587, #2856 ) ;
#5543 = VERTEX_POINT ( 'NONE', #1484 ) ;
#5544 = FACE_OUTER_BOUND ( 'NONE', #1771, .T. ) ;
#5545 = DIRECTION ( 'NONE',  ( 1.000000000000000000, 2.220446049250313870E-15, 4.237045877651953088E-33 ) ) ;
#5546 = ORIENTED_EDGE ( 'NONE', *, *, #5395, .F. ) ;
#5547 = AXIS2_PLACEMENT_3D ( 'NONE', #7235, #1199, #625 ) ;
#5548 = CARTESIAN_POINT ( 'NONE',  ( 25.00000000000002132, 36.67766952966366745, 4.535533905932717325 ) ) ;
#5549 = CARTESIAN_POINT ( 'NONE',  ( 25.00000000000000711, 28.00000000000002487, 9.999999999999996447 ) ) ;
#5550 = EDGE_CURVE ( 'NONE', #1572, #1226, #417, .T. ) ;
#5551 = ORIENTED_EDGE ( 'NONE', *, *, #5829, .T. ) ;
#5552 = AXIS2_PLACEMENT_3D ( 'NONE', #5453, #5418, #6570 ) ;
#5553 = DIRECTION ( 'NONE',  ( -1.000000000000000000, 0.000000000000000000, -7.663350976776343357E-46 ) ) ;
#5554 = CYLINDRICAL_SURFACE ( 'NONE', #6183, 8.000000000000017764 ) ;
#5555 = CARTESIAN_POINT ( 'NONE',  ( 220.0000000000000000, -15.08392021690038121, 12.00000000000000711 ) ) ;
#5556 = ORIENTED_EDGE ( 'NONE', *, *, #636, .T. ) ;
#5557 =( NAMED_UNIT ( * ) SI_UNIT ( $, .STERADIAN. ) SOLID_ANGLE_UNIT ( ) );
#5558 = AXIS2_PLACEMENT_3D ( 'NONE', #2607, #1525, #2649 ) ;
#5559 = CARTESIAN_POINT ( 'NONE',  ( 47.00000000000000000, 21.91628335801839356, 36.91742634044857141 ) ) ;
#5560 = CARTESIAN_POINT ( 'NONE',  ( 3.000000000000002665, 60.00000000000000000, 3.000000000000021760 ) ) ;
#5561 = DIRECTION ( 'NONE',  ( -5.605193857299270773E-45, -0.000000000000000000, -1.000000000000000000 ) ) ;
#5562 = EDGE_CURVE ( 'NONE', #5749, #3892, #7265, .T. ) ;
#5563 = VERTEX_POINT ( 'NONE', #1451 ) ;
#5564 = ORIENTED_EDGE ( 'NONE', *, *, #1642, .F. ) ;
#5565 = LINE ( 'NONE', #974, #7211 ) ;
#5566 = DIRECTION ( 'NONE',  ( -0.000000000000000000, -0.000000000000000000, 1.000000000000000000 ) ) ;
#5567 = CARTESIAN_POINT ( 'NONE',  ( 216.9999999999999716, 6.000000000000000000, 35.00000000000000000 ) ) ;
#5568 = CARTESIAN_POINT ( 'NONE',  ( -61.18228816775778256, -223.0630240738406087, 76.64217870502731955 ) ) ;
#5569 = DIRECTION ( 'NONE',  ( 0.000000000000000000, 0.000000000000000000, 1.000000000000000000 ) ) ;
#5570 = DIRECTION ( 'NONE',  ( 0.000000000000000000, 0.000000000000000000, -1.000000000000000000 ) ) ;
#5571 = ORIENTED_EDGE ( 'NONE', *, *, #5209, .T. ) ;
#5572 = ORIENTED_EDGE ( 'NONE', *, *, #4174, .T. ) ;
#5573 = ADVANCED_FACE ( 'NONE', ( #1992 ), #5615, .T. ) ;
#5574 = DIRECTION ( 'NONE',  ( 0.000000000000000000, 0.000000000000000000, 1.000000000000000000 ) ) ;
#5575 = CYLINDRICAL_SURFACE ( 'NONE', #2028, 13.99999999999999645 ) ;
#5576 = LINE ( 'NONE', #5504, #1612 ) ;
#5577 = CIRCLE ( 'NONE', #4728, 14.00000000000000533 ) ;
#5578 = ORIENTED_EDGE ( 'NONE', *, *, #983, .F. ) ;
#5579 = VERTEX_POINT ( 'NONE', #6112 ) ;
#5580 = AXIS2_PLACEMENT_3D ( 'NONE', #349, #3284, #4985 ) ;
#5581 = ADVANCED_FACE ( 'NONE', ( #5036 ), #5575, .F. ) ;
#5582=STYLED_ITEM('',(#7624),#6277);
#5583 = FACE_OUTER_BOUND ( 'NONE', #1405, .T. ) ;
#5584 = ORIENTED_EDGE ( 'NONE', *, *, #2936, .T. ) ;
#5585 = LINE ( 'NONE', #1382, #3212 ) ;
#5586 = CARTESIAN_POINT ( 'NONE',  ( 2.000000000000001776, 1.224646799147353651E-15, 10.00000000000000355 ) ) ;
#5587 = AXIS2_PLACEMENT_3D ( 'NONE', #1531, #6229, #958 ) ;
#5588=STYLED_ITEM('',(#7652),#6414);
#5589 = VECTOR ( 'NONE', #6855, 1000.000000000000000 ) ;
#5590 = ORIENTED_EDGE ( 'NONE', *, *, #1442, .F. ) ;
#5591 = DIRECTION ( 'NONE',  ( -1.000000000000000000, -0.000000000000000000, -0.000000000000000000 ) ) ;
#5592 = AXIS2_PLACEMENT_3D ( 'NONE', #6799, #3306, #411 ) ;
#5593 = VECTOR ( 'NONE', #6216, 1000.000000000000000 ) ;
#5594 = EDGE_CURVE ( 'NONE', #4559, #5270, #2642, .T. ) ;
#5595 = CARTESIAN_POINT ( 'NONE',  ( 188.4942707396337482, 3.000000000000000000, 17.75098426722491851 ) ) ;
#5596 = DIRECTION ( 'NONE',  ( 1.000000000000000000, 0.000000000000000000, 0.000000000000000000 ) ) ;
#5597 = VECTOR ( 'NONE', #7291, 1000.000000000000000 ) ;
#5598 = VERTEX_POINT ( 'NONE', #2036 ) ;
#5599 = CARTESIAN_POINT ( 'NONE',  ( -60.75187451922243298, -218.1519544391847489, 95.22527181742795221 ) ) ;
#5600 = CARTESIAN_POINT ( 'NONE',  ( 188.0000000000000000, -14.00000000000000711, -7.000000000000017764 ) ) ;
#5601 =( NAMED_UNIT ( * ) PLANE_ANGLE_UNIT ( ) SI_UNIT ( $, .RADIAN. ) );
#5602 = EDGE_LOOP ( 'NONE', ( #1274, #2088, #5261, #490 ) ) ;
#5603 = ORIENTED_EDGE ( 'NONE', *, *, #6472, .T. ) ;
#5604 = FACE_OUTER_BOUND ( 'NONE', #3956, .T. ) ;
#5605 = EDGE_CURVE ( 'NONE', #2502, #5312, #6694, .T. ) ;
#5606 = LINE ( 'NONE', #5140, #3629 ) ;
#5607 = DIRECTION ( 'NONE',  ( 0.000000000000000000, 1.000000000000000000, 0.000000000000000000 ) ) ;
#5608 = FACE_OUTER_BOUND ( 'NONE', #7043, .T. ) ;
#5609 = CARTESIAN_POINT ( 'NONE',  ( 185.0000000000000000, -39.99999999999999289, 0.000000000000000000 ) ) ;
#5610 = PLANE ( 'NONE',  #6639 ) ;
#5611 = VERTEX_POINT ( 'NONE', #3771 ) ;
#5612 = CIRCLE ( 'NONE', #7083, 2.999999999999999112 ) ;
#5613 = VERTEX_POINT ( 'NONE', #5464 ) ;
#5614 = FACE_OUTER_BOUND ( 'NONE', #5196, .T. ) ;
#5615 = CYLINDRICAL_SURFACE ( 'NONE', #1407, 3.000000000000000444 ) ;
#5616 = FACE_OUTER_BOUND ( 'NONE', #6558, .T. ) ;
#5617 = ORIENTED_EDGE ( 'NONE', *, *, #4429, .T. ) ;
#5618 = ORIENTED_EDGE ( 'NONE', *, *, #1998, .F. ) ;
#5619 = VECTOR ( 'NONE', #6372, 1000.000000000000000 ) ;
#5620 = CARTESIAN_POINT ( 'NONE',  ( 50.00000000000000000, -17.97033316447826579, 12.83599132585211322 ) ) ;
#5621 = ORIENTED_EDGE ( 'NONE', *, *, #7463, .T. ) ;
#5622 = DIRECTION ( 'NONE',  ( 0.000000000000000000, 0.000000000000000000, -1.000000000000000000 ) ) ;
#5623 = CARTESIAN_POINT ( 'NONE',  ( -16.49999999999996447, -45.34314575050758123, 18.34314575050765939 ) ) ;
#5624 = EDGE_CURVE ( 'NONE', #4630, #5613, #5714, .T. ) ;
#5625 = ORIENTED_EDGE ( 'NONE', *, *, #7493, .T. ) ;
#5626 = CARTESIAN_POINT ( 'NONE',  ( 48.84364016120485275, 26.43524405526845200, 12.79091332731197461 ) ) ;
#5627 = CARTESIAN_POINT ( 'NONE',  ( 217.0000000000000000, -9.000000000000001776, 18.00000000000001066 ) ) ;
#5628 = ORIENTED_EDGE ( 'NONE', *, *, #6378, .F. ) ;
#5629 = CARTESIAN_POINT ( 'NONE',  ( -53.25365409304695419, -218.1074892565148389, 95.21743140602109179 ) ) ;
#5630 = DIRECTION ( 'NONE',  ( -1.000000000000000000, 0.000000000000000000, 0.000000000000000000 ) ) ;
#5631 = CARTESIAN_POINT ( 'NONE',  ( 201.3397459621555470, -3.000000000000000888, 39.99999999999999289 ) ) ;
#5632 = EDGE_CURVE ( 'NONE', #6935, #2502, #835, .T. ) ;
#5633 = ORIENTED_EDGE ( 'NONE', *, *, #5796, .T. ) ;
#5634 = ORIENTED_EDGE ( 'NONE', *, *, #1376, .T. ) ;
#5635 = LINE ( 'NONE', #3798, #698 ) ;
#5636 = CARTESIAN_POINT ( 'NONE',  ( 26.00000000000000000, 7.347880794883831802E-16, -6.000000000000000888 ) ) ;
#5637 = CARTESIAN_POINT ( 'NONE',  ( -53.03180245857092956, -218.0630240738404950, 71.94153218116483117 ) ) ;
#5638 = CARTESIAN_POINT ( 'NONE',  ( -21.50000000000000000, -69.31370849898461017, 42.31370849898474518 ) ) ;
#5639 = CARTESIAN_POINT ( 'NONE',  ( 49.99999999999998579, -25.78715168812825098, 12.89530150989249435 ) ) ;
#5640 = CARTESIAN_POINT ( 'NONE',  ( -16.47169665601479949, -116.3958977277557523, 43.92260702357706492 ) ) ;
#5641 = DIRECTION ( 'NONE',  ( 0.000000000000000000, -1.000000000000000000, 0.000000000000000000 ) ) ;
#5642 = EDGE_CURVE ( 'NONE', #4912, #6424, #2071, .T. ) ;
#5643 = EDGE_CURVE ( 'NONE', #5778, #920, #1409, .T. ) ;
#5644 = ORIENTED_EDGE ( 'NONE', *, *, #962, .T. ) ;
#5645 = VERTEX_POINT ( 'NONE', #3149 ) ;
#5646 = DIRECTION ( 'NONE',  ( -1.000000000000000000, 0.000000000000000000, -7.663350976776343357E-46 ) ) ;
#5647 = CARTESIAN_POINT ( 'NONE',  ( 21.50000000000000000, -105.5631177942458265, 67.24940929526127320 ) ) ;
#5648 = DIRECTION ( 'NONE',  ( 0.000000000000000000, -0.9860132971832693549, 0.1666666666666667684 ) ) ;
#5649 = CARTESIAN_POINT ( 'NONE',  ( -10.49999999999997513, -104.2695387347598057, 32.26953873475996204 ) ) ;
#5650 = VECTOR ( 'NONE', #3951, 1000.000000000000000 ) ;
#5651 = ADVANCED_FACE ( 'NONE', ( #4578 ), #6259, .F. ) ;
#5652 = ORIENTED_EDGE ( 'NONE', *, *, #5796, .F. ) ;
#5653 = ORIENTED_EDGE ( 'NONE', *, *, #4853, .F. ) ;
#5654 = CIRCLE ( 'NONE', #2952, 6.000000000000019540 ) ;
#5655 = VECTOR ( 'NONE', #1258, 1000.000000000000000 ) ;
#5656 = DIRECTION ( 'NONE',  ( 0.000000000000000000, 0.000000000000000000, -1.000000000000000000 ) ) ;
#5657 = VERTEX_POINT ( 'NONE', #6384 ) ;
#5658 = CARTESIAN_POINT ( 'NONE',  ( 26.99999999999999289, 0.000000000000000000, -9.999999999999994671 ) ) ;
#5659 = DIRECTION ( 'NONE',  ( -2.465190328815661892E-32, -1.000000000000000000, -1.193489751472043281E-15 ) ) ;
#5660 = AXIS2_PLACEMENT_3D ( 'NONE', #324, #6130, #4374 ) ;
#5661 = VERTEX_POINT ( 'NONE', #487 ) ;
#5662 = ADVANCED_FACE ( 'NONE', ( #3430 ), #5190, .F. ) ;
#5663 = VECTOR ( 'NONE', #6151, 1000.000000000000000 ) ;
#5664 = CYLINDRICAL_SURFACE ( 'NONE', #176, 3.000000000000000000 ) ;
#5665 = CARTESIAN_POINT ( 'NONE',  ( -29.50000000000000000, -223.0630240738404950, 73.28127814332044920 ) ) ;
#5666 = ORIENTED_EDGE ( 'NONE', *, *, #609, .F. ) ;
#5667 = DIRECTION ( 'NONE',  ( 3.352817876578150312E-29, 0.8774352413474597601, 0.4796951086278917753 ) ) ;
#5668 = CARTESIAN_POINT ( 'NONE',  ( -13.49999999999999822, -215.0630240738404382, 73.28127814332047762 ) ) ;
#5669 = DIRECTION ( 'NONE',  ( 0.4999999999999976685, 0.000000000000000000, 0.8660254037844400399 ) ) ;
#5670 = ORIENTED_EDGE ( 'NONE', *, *, #4786, .F. ) ;
#5671 = ORIENTED_EDGE ( 'NONE', *, *, #6532, .F. ) ;
#5672 = AXIS2_PLACEMENT_3D ( 'NONE', #7178, #5380, #3653 ) ;
#5673 = EDGE_CURVE ( 'NONE', #640, #6429, #1522, .T. ) ;
#5674 = CARTESIAN_POINT ( 'NONE',  ( -26.99999999999999289, 3.306546357697851761E-15, -9.999999999999994671 ) ) ;
#5675 = DIRECTION ( 'NONE',  ( -6.162975822039153361E-33, -5.166928274020107963E-17, 1.000000000000000000 ) ) ;
#5676 = EDGE_CURVE ( 'NONE', #2698, #1052, #677, .T. ) ;
#5677 = CARTESIAN_POINT ( 'NONE',  ( -16.49999999999996447, 0.000000000000000000, 0.000000000000000000 ) ) ;
#5678 = CARTESIAN_POINT ( 'NONE',  ( -57.86411036119383056, -223.0630208489766915, 95.16303203405658451 ) ) ;
#5679 = DIRECTION ( 'NONE',  ( 1.000000000000000000, -0.000000000000000000, -0.000000000000000000 ) ) ;
#5680 = CARTESIAN_POINT ( 'NONE',  ( 0.000000000000000000, 1.714505518806293455E-15, 21.00000000000001066 ) ) ;
#5681 = LINE ( 'NONE', #404, #5831 ) ;
#5682 = AXIS2_PLACEMENT_3D ( 'NONE', #6800, #3187, #3152 ) ;
#5683 =( BOUNDED_SURFACE ( )  B_SPLINE_SURFACE ( 3, 2, ( 
 ( #6125, #3204, #280 ),
 ( #2731, #4403, #1463 ),
 ( #849, #1537, #6741 ),
 ( #2622, #1497, #3861 ),
 ( #6195, #4224, #5626 ),
 ( #3901, #5087, #6569 ),
 ( #2010, #3652, #5992 ),
 ( #4944, #4369, #6854 ),
 ( #1083, #1660, #1574 ),
 ( #6275, #2893, #7009 ) ),
 .UNSPECIFIED., .F., .F., .T. ) 
 B_SPLINE_SURFACE_WITH_KNOTS ( ( 4, 2, 2, 2, 4 ),
 ( 3, 3 ),
 ( 0.000000000000000000, 0.3926990816987241395, 0.7853981633974482790, 1.178097245096172418, 1.570796326794896558 ),
 ( 0.000000000000000000, 1.000000000000000000 ),
 .UNSPECIFIED. ) 
 GEOMETRIC_REPRESENTATION_ITEM ( )  RATIONAL_B_SPLINE_SURFACE ( (
 ( 1.000000000000000000, 0.7372773368101256386, 1.000000000000000000),
 ( 1.000000000000000000, 0.7372805249393075133, 1.000000000000000000),
 ( 1.000000000000000000, 0.7365092403365430807, 1.000000000000000000),
 ( 1.000000000000000000, 0.7335393349597864043, 1.000000000000000000),
 ( 1.000000000000000000, 0.7313381170114944263, 1.000000000000000000),
 ( 1.000000000000000000, 0.7258018328328726954, 1.000000000000000000),
 ( 1.000000000000000000, 0.7224680490849620940, 1.000000000000000000),
 ( 1.000000000000000000, 0.7151362488948415086, 1.000000000000000000),
 ( 1.000000000000000000, 0.7111416486853837648, 1.000000000000000000),
 ( 1.000000000000000000, 0.7071067811865475727, 1.000000000000000000) ) ) 
 REPRESENTATION_ITEM ( '' )  SURFACE ( )  );
#5684 = VERTEX_POINT ( 'NONE', #7527 ) ;
#5685 = ORIENTED_EDGE ( 'NONE', *, *, #2314, .F. ) ;
#5686 = DIRECTION ( 'NONE',  ( 1.000000000000000000, 0.000000000000000000, 0.000000000000000000 ) ) ;
#5687 = DIRECTION ( 'NONE',  ( 1.000000000000000000, -0.000000000000000000, -0.000000000000000000 ) ) ;
#5688 = LINE ( 'NONE', #2758, #6081 ) ;
#5689 = CARTESIAN_POINT ( 'NONE',  ( 25.00000000000001421, 80.85786437626907741, 8.071067811865434649 ) ) ;
#5690 = EDGE_CURVE ( 'NONE', #6366, #3365, #1638, .T. ) ;
#5691 = CARTESIAN_POINT ( 'NONE',  ( 3.000000000000002665, -25.78715168812825098, 12.89530150989249435 ) ) ;
#5692 = VERTEX_POINT ( 'NONE', #3462 ) ;
#5693 = VERTEX_POINT ( 'NONE', #7411 ) ;
#5694 = CYLINDRICAL_SURFACE ( 'NONE', #6937, 10.00000000000000355 ) ;
#5695 = ADVANCED_FACE ( 'NONE', ( #2801 ), #7309, .T. ) ;
#5696 = VERTEX_POINT ( 'NONE', #4457 ) ;
#5697 = DIRECTION ( 'NONE',  ( -0.000000000000000000, -0.000000000000000000, 1.000000000000000000 ) ) ;
#5698 = CARTESIAN_POINT ( 'NONE',  ( 53.00000000000000711, -20.99999999999999645, 10.00000000000000888 ) ) ;
#5699 = ADVANCED_FACE ( 'NONE', ( #1563 ), #5805, .T. ) ;
#5700 = EDGE_LOOP ( 'NONE', ( #2153, #468, #5348, #4935 ) ) ;
#5701 = CIRCLE ( 'NONE', #1515, 4.999999999999999112 ) ;
#5702 = CIRCLE ( 'NONE', #3741, 5.000000000000004441 ) ;
#5703 = CARTESIAN_POINT ( 'NONE',  ( 50.00000000000000000, 0.000000000000000000, 48.99999999999999289 ) ) ;
#5704 = DIRECTION ( 'NONE',  ( 5.605193857299270773E-45, 0.000000000000000000, 1.000000000000000000 ) ) ;
#5705 = VERTEX_POINT ( 'NONE', #5118 ) ;
#5706 = CYLINDRICAL_SURFACE ( 'NONE', #3222, 7.999999999999986677 ) ;
#5707 = AXIS2_PLACEMENT_3D ( 'NONE', #1911, #4841, #6063 ) ;
#5708 = SPHERICAL_SURFACE ( 'NONE', #6762, 3.000000000000000000 ) ;
#5709 = VECTOR ( 'NONE', #4898, 1000.000000000000000 ) ;
#5710 = DIRECTION ( 'NONE',  ( 0.000000000000000000, -1.000000000000000000, -3.304235192336776498E-16 ) ) ;
#5711 = ORIENTED_EDGE ( 'NONE', *, *, #6993, .F. ) ;
#5712 = EDGE_LOOP ( 'NONE', ( #5892, #1593, #3532, #3964, #5433, #1088, #474, #24 ) ) ;
#5713 = EDGE_CURVE ( 'NONE', #6714, #5322, #5960, .T. ) ;
#5714 = CIRCLE ( 'NONE', #1041, 8.000000000000003553 ) ;
#5715 = VECTOR ( 'NONE', #4528, 1000.000000000000000 ) ;
#5716 = AXIS2_PLACEMENT_3D ( 'NONE', #2414, #3537, #1217 ) ;
#5717 = CARTESIAN_POINT ( 'NONE',  ( -21.35140889653590790, -111.8253808406378624, 39.82538084063802586 ) ) ;
#5718 = PRESENTATION_STYLE_ASSIGNMENT (( #3295 ) ) ;
#5719 = DIRECTION ( 'NONE',  ( 0.000000000000000000, -0.9993908270190955401, 0.03489949670250346025 ) ) ;
#5720 = CARTESIAN_POINT ( 'NONE',  ( -61.39066111053622166, -223.0630240738405234, 92.67132228217317902 ) ) ;
#5721 = LINE ( 'NONE', #365, #251 ) ;
#5722 = CARTESIAN_POINT ( 'NONE',  ( 40.00000000000000000, -4.163336342344337027E-14, 1.387778780781445676E-14 ) ) ;
#5723 = VECTOR ( 'NONE', #4013, 1000.000000000000000 ) ;
#5725 = LINE ( 'NONE', #4472, #785 ) ;
#5724 =( GEOMETRIC_REPRESENTATION_CONTEXT ( 3 ) GLOBAL_UNCERTAINTY_ASSIGNED_CONTEXT ( ( #637 ) ) GLOBAL_UNIT_ASSIGNED_CONTEXT ( ( #5446, #3064, #4291 ) ) REPRESENTATION_CONTEXT ( 'NONE', 'WORKASPACE' ) );
#5726 = EDGE_LOOP ( 'NONE', ( #4445, #56, #3795, #907 ) ) ;
#5727 = VERTEX_POINT ( 'NONE', #6221 ) ;
#5728 = CARTESIAN_POINT ( 'NONE',  ( 47.00000000000000000, 30.03170604878415162, 10.00000000000001243 ) ) ;
#5729 = CARTESIAN_POINT ( 'NONE',  ( 192.1021416551216419, -6.000000000000000888, 18.00000000000001066 ) ) ;
#5730 = DIRECTION ( 'NONE',  ( 1.000000000000000000, 0.000000000000000000, 0.000000000000000000 ) ) ;
#5731 = CARTESIAN_POINT ( 'NONE',  ( -24.15685424949240456, -63.34314575050749596, 36.34314575050759544 ) ) ;
#5732 = DIRECTION ( 'NONE',  ( -0.000000000000000000, -0.000000000000000000, 1.000000000000000000 ) ) ;
#5733 = DIRECTION ( 'NONE',  ( 1.381786968815111140E-76, -1.000000000000000000, -1.221245327087672392E-15 ) ) ;
#5734 = VECTOR ( 'NONE', #3111, 1000.000000000000114 ) ;
#5735 = ORIENTED_EDGE ( 'NONE', *, *, #3912, .T. ) ;
#5736 = EDGE_CURVE ( 'NONE', #868, #5355, #306, .T. ) ;
#5737 = VERTEX_POINT ( 'NONE', #5689 ) ;
#5738 = FACE_BOUND ( 'NONE', #7492, .T. ) ;
#5739 = VECTOR ( 'NONE', #641, 1000.000000000000000 ) ;
#5740 = CARTESIAN_POINT ( 'NONE',  ( 25.00000000000000000, 12.49999999999998401, 4.999999999999995559 ) ) ;
#5741 = CARTESIAN_POINT ( 'NONE',  ( 0.000000000000000000, 0.000000000000000000, -39.99999999999997868 ) ) ;
#5742 = CARTESIAN_POINT ( 'NONE',  ( 21.50000000000000000, -223.0630240738404666, 96.09122589815579829 ) ) ;
#5743 = VERTEX_POINT ( 'NONE', #1685 ) ;
#5744 = VECTOR ( 'NONE', #3094, 1000.000000000000000 ) ;
#5745 = EDGE_CURVE ( 'NONE', #584, #3, #4617, .T. ) ;
#5746 = ADVANCED_FACE ( 'NONE', ( #4041 ), #7565, .F. ) ;
#5747 = CARTESIAN_POINT ( 'NONE',  ( 3.000000000000002665, -18.00000000000000000, 7.000000000000008882 ) ) ;
#5748 = FACE_BOUND ( 'NONE', #4787, .T. ) ;
#5749 = VERTEX_POINT ( 'NONE', #375 ) ;
#5750 = AXIS2_PLACEMENT_3D ( 'NONE', #6466, #4701, #5812 ) ;
#5751 = DIRECTION ( 'NONE',  ( 1.000000000000000000, 2.465190328815661892E-32, -9.244463733058732095E-33 ) ) ;
#5752 = CARTESIAN_POINT ( 'NONE',  ( 4.000000000000003553, 0.000000000000000000, 10.00000000000001243 ) ) ;
#5753 = CARTESIAN_POINT ( 'NONE',  ( -31.48397095257174527, -63.85254959896236215, 36.85254959896246874 ) ) ;
#5754 = ORIENTED_EDGE ( 'NONE', *, *, #5562, .T. ) ;
#5755 = VERTEX_POINT ( 'NONE', #5072 ) ;
#5756 = FACE_OUTER_BOUND ( 'NONE', #1448, .T. ) ;
#5757 = CARTESIAN_POINT ( 'NONE',  ( 188.2878511289427195, 5.841022112857982229, 17.39345501382462444 ) ) ;
#5758 = DIRECTION ( 'NONE',  ( -1.000000000000000000, 0.000000000000000000, 1.445602896647337931E-16 ) ) ;
#5759 = CARTESIAN_POINT ( 'NONE',  ( 17.65194526459429625, -223.0630240738404098, 76.13224682984757408 ) ) ;
#5760 = PLANE ( 'NONE',  #3691 ) ;
#5761 = PRODUCT_DEFINITION_SHAPE ( 'NONE', 'NONE',  #7604 ) ;
#5762 = CARTESIAN_POINT ( 'NONE',  ( -63.27290876320206081, -218.0630240738404666, 78.35050765050191046 ) ) ;
#5763 = ORIENTED_EDGE ( 'NONE', *, *, #2968, .F. ) ;
#5764 = DIRECTION ( 'NONE',  ( -1.000000000000000000, 0.000000000000000000, 0.000000000000000000 ) ) ;
#5765 = DIRECTION ( 'NONE',  ( 0.000000000000000000, -1.000000000000000000, -1.836970198721029934E-16 ) ) ;
#5766 = CARTESIAN_POINT ( 'NONE',  ( 0.000000000000000000, 24.05453786023368323, 12.47706554351403874 ) ) ;
#5767 = EDGE_CURVE ( 'NONE', #6160, #3744, #2757, .T. ) ;
#5768 = CARTESIAN_POINT ( 'NONE',  ( 3.000000000000000000, 21.91628335801839711, 36.91742634044857141 ) ) ;
#5769 = CARTESIAN_POINT ( 'NONE',  ( 188.6380400399839061, -9.000000000000001776, 15.00000000000001066 ) ) ;
#5770 = ORIENTED_EDGE ( 'NONE', *, *, #1487, .F. ) ;
#5771 = ORIENTED_EDGE ( 'NONE', *, *, #3101, .F. ) ;
#5772 = CARTESIAN_POINT ( 'NONE',  ( -18.84314575050759188, -108.3431457505073752, 36.34314575050756702 ) ) ;
#5773 = ADVANCED_FACE ( 'NONE', ( #2148 ), #4503, .T. ) ;
#5774 = FACE_OUTER_BOUND ( 'NONE', #6502, .T. ) ;
#5775 = ORIENTED_EDGE ( 'NONE', *, *, #2916, .T. ) ;
#5776 = CARTESIAN_POINT ( 'NONE',  ( 52.84383605861879829, -24.35311149449081825, 10.00000000000000888 ) ) ;
#5777 = LINE ( 'NONE', #7085, #3119 ) ;
#5778 = VERTEX_POINT ( 'NONE', #6572 ) ;
#5779 = CIRCLE ( 'NONE', #2, 3.000000000000000888 ) ;
#5780 = EDGE_LOOP ( 'NONE', ( #3433, #4172, #6425 ) ) ;
#5781 = TOROIDAL_SURFACE ( 'NONE', #2459, 7.000000000000019540, 3.000000000000000000 ) ;
#5782 = DIRECTION ( 'NONE',  ( -1.000000000000000000, 5.551115123125783935E-17, -4.237045877651919561E-33 ) ) ;
#5783 = CARTESIAN_POINT ( 'NONE',  ( 17.68960140267981984, -213.9340789708221564, 94.48154657109715515 ) ) ;
#5784 = ORIENTED_EDGE ( 'NONE', *, *, #2353, .F. ) ;
#5785 = AXIS2_PLACEMENT_3D ( 'NONE', #2735, #5630, #3939 ) ;
#5786 = EDGE_CURVE ( 'NONE', #2821, #3936, #426, .T. ) ;
#5787 = CARTESIAN_POINT ( 'NONE',  ( 220.0000000000000000, 15.08392021690038121, 12.00000000000000711 ) ) ;
#5788 = DIRECTION ( 'NONE',  ( -1.000000000000000000, -2.465190328815661892E-32, -9.244463733058733463E-33 ) ) ;
#5789 = VERTEX_POINT ( 'NONE', #1180 ) ;
#5790 = ORIENTED_EDGE ( 'NONE', *, *, #4461, .F. ) ;
#5791 = AXIS2_PLACEMENT_3D ( 'NONE', #4855, #2461, #7084 ) ;
#5792 = FACE_OUTER_BOUND ( 'NONE', #6552, .T. ) ;
#5793 = CARTESIAN_POINT ( 'NONE',  ( 2.000000000000001776, -4.163336342344337027E-14, 0.000000000000000000 ) ) ;
#5794 = CARTESIAN_POINT ( 'NONE',  ( 189.3200985330552726, 7.169359205023974724, 15.59067998186761095 ) ) ;
#5795 = CARTESIAN_POINT ( 'NONE',  ( 21.49983462661594658, -218.0630240738406087, 83.89749897642222720 ) ) ;
#5796 = EDGE_CURVE ( 'NONE', #6417, #3729, #6872, .T. ) ;
#5797 = CARTESIAN_POINT ( 'NONE',  ( 17.23587211895880955, -223.0630240738404098, 75.76440619659675235 ) ) ;
#5798 = PLANE ( 'NONE',  #3933 ) ;
#5799 = CARTESIAN_POINT ( 'NONE',  ( -63.67751884086511893, -218.0631193926485309, 79.33280772544384263 ) ) ;
#5800 = UNCERTAINTY_MEASURE_WITH_UNIT (LENGTH_MEASURE( 1.000000000000000082E-05 ), #6568, 'distance_accuracy_value', 'NONE');
#5801 = EDGE_LOOP ( 'NONE', ( #4087, #4526, #4812, #2006 ) ) ;
#5802 = LINE ( 'NONE', #4615, #3120 ) ;
#5803 = DIRECTION ( 'NONE',  ( 0.000000000000000000, 0.000000000000000000, 1.000000000000000000 ) ) ;
#5804 = DIRECTION ( 'NONE',  ( 0.000000000000000000, 0.000000000000000000, -1.000000000000000000 ) ) ;
#5805 = SPHERICAL_SURFACE ( 'NONE', #1655, 3.000000000000000000 ) ;
#5806 = DIRECTION ( 'NONE',  ( -1.000000000000000000, -2.624548829666596736E-30, 9.231085635203017994E-31 ) ) ;
#5807 = VECTOR ( 'NONE', #1603, 1000.000000000000000 ) ;
#5808 = ORIENTED_EDGE ( 'NONE', *, *, #2261, .T. ) ;
#5809 = EDGE_CURVE ( 'NONE', #3515, #2618, #5702, .T. ) ;
#5810 = ORIENTED_EDGE ( 'NONE', *, *, #2708, .T. ) ;
#5811 = EDGE_CURVE ( 'NONE', #3264, #1631, #5577, .T. ) ;
#5812 = DIRECTION ( 'NONE',  ( -1.000000000000000000, 0.000000000000000000, 0.000000000000000000 ) ) ;
#5813 = DIRECTION ( 'NONE',  ( -0.000000000000000000, -0.000000000000000000, 1.000000000000000000 ) ) ;
#5814 = ORIENTED_EDGE ( 'NONE', *, *, #5414, .T. ) ;
#5815 = CARTESIAN_POINT ( 'NONE',  ( -21.49999999999999645, -125.0933926253236450, 30.46597562735434295 ) ) ;
#5816 = CARTESIAN_POINT ( 'NONE',  ( 217.0000000000000000, -56.99999999999999289, 3.000000000000000444 ) ) ;
#5817 = ORIENTED_EDGE ( 'NONE', *, *, #3868, .T. ) ;
#5818 = EDGE_CURVE ( 'NONE', #2858, #3174, #4598, .T. ) ;
#5819 = ORIENTED_EDGE ( 'NONE', *, *, #4151, .T. ) ;
#5820 = DIRECTION ( 'NONE',  ( 0.000000000000000000, -1.000000000000000000, -2.065146995210484941E-16 ) ) ;
#5821 = DIRECTION ( 'NONE',  ( 1.000000000000000000, 0.000000000000000000, 0.000000000000000000 ) ) ;
#5822 = ORIENTED_EDGE ( 'NONE', *, *, #3382, .F. ) ;
#5823 = PRODUCT_CONTEXT ( 'NONE', #1916, 'mechanical' ) ;
#5824 = CARTESIAN_POINT ( 'NONE',  ( 192.1021416551216419, -6.000000000000000000, 18.00000000000001066 ) ) ;
#5825 = DIRECTION ( 'NONE',  ( -0.000000000000000000, 1.000000000000000000, 3.304235192336776498E-16 ) ) ;
#5826 = CIRCLE ( 'NONE', #4470, 6.000000000000019540 ) ;
#5827 = ORIENTED_EDGE ( 'NONE', *, *, #3200, .F. ) ;
#5828 = EDGE_CURVE ( 'NONE', #4634, #1071, #6536, .T. ) ;
#5829 = EDGE_CURVE ( 'NONE', #5113, #1919, #2994, .T. ) ;
#5830 = CARTESIAN_POINT ( 'NONE',  ( -21.48215622306531003, -113.7796841263388501, 41.77968412633906325 ) ) ;
#5831 = VECTOR ( 'NONE', #3377, 1000.000000000000000 ) ;
#5832 = VECTOR ( 'NONE', #2716, 1000.000000000000114 ) ;
#5833 = DIRECTION ( 'NONE',  ( -1.000000000000000000, -2.624548829666596736E-30, 9.231085635203017994E-31 ) ) ;
#5834 = AXIS2_PLACEMENT_3D ( 'NONE', #2586, #3132, #4906 ) ;
#5835 = CARTESIAN_POINT ( 'NONE',  ( 16.32211914470424574, -218.0630240738405519, 93.45296875943058978 ) ) ;
#5836 = LINE ( 'NONE', #558, #6638 ) ;
#5837 = LINE ( 'NONE', #4068, #6880 ) ;
#5838 = VECTOR ( 'NONE', #5013, 1000.000000000000000 ) ;
#5839 =( GEOMETRIC_REPRESENTATION_CONTEXT ( 3 ) GLOBAL_UNCERTAINTY_ASSIGNED_CONTEXT ( ( #6144 ) ) GLOBAL_UNIT_ASSIGNED_CONTEXT ( ( #6028, #1945, #2023 ) ) REPRESENTATION_CONTEXT ( 'NONE', 'WORKASPACE' ) );
#5840 = EDGE_CURVE ( 'NONE', #6366, #3524, #2083, .T. ) ;
#5841 = ORIENTED_EDGE ( 'NONE', *, *, #4544, .T. ) ;
#5842 = PRESENTATION_STYLE_ASSIGNMENT (( #3494 ) ) ;
#5843 = LINE ( 'NONE', #5265, #151 ) ;
#5844 = DIRECTION ( 'NONE',  ( 0.000000000000000000, 0.000000000000000000, 1.000000000000000000 ) ) ;
#5845 = DIRECTION ( 'NONE',  ( 1.000000000000000000, -5.551115123125783935E-17, 4.237045877651919561E-33 ) ) ;
#5846 = AXIS2_PLACEMENT_3D ( 'NONE', #1316, #3675, #4870 ) ;
#5847 = AXIS2_PLACEMENT_3D ( 'NONE', #4695, #5381, #5844 ) ;
#5848 = CARTESIAN_POINT ( 'NONE',  ( 209.9999999999999716, -6.000000000000000000, 35.00000000000000000 ) ) ;
#5849 = ORIENTED_EDGE ( 'NONE', *, *, #7107, .T. ) ;
#5850 = AXIS2_PLACEMENT_3D ( 'NONE', #932, #967, #391 ) ;
#5851 = ORIENTED_EDGE ( 'NONE', *, *, #5920, .F. ) ;
#5852 = CYLINDRICAL_SURFACE ( 'NONE', #5384, 12.49999999999999467 ) ;
#5853 = CARTESIAN_POINT ( 'NONE',  ( 4.000000000000000000, 1.224646799147353651E-15, -10.00000000000000355 ) ) ;
#5854 = ORIENTED_EDGE ( 'NONE', *, *, #3641, .F. ) ;
#5855 = DIRECTION ( 'NONE',  ( 1.000000000000000000, 0.000000000000000000, 0.000000000000000000 ) ) ;
#5856 = LINE ( 'NONE', #7001, #4620 ) ;
#5857 = ORIENTED_EDGE ( 'NONE', *, *, #3301, .F. ) ;
#5858 = VERTEX_POINT ( 'NONE', #719 ) ;
#5859 = AXIS2_PLACEMENT_3D ( 'NONE', #5071, #4389, #6798 ) ;
#5860 = CARTESIAN_POINT ( 'NONE',  ( -32.50000000000002842, -49.37258300203047412, -6.000000000000002665 ) ) ;
#5861 = CARTESIAN_POINT ( 'NONE',  ( 17.75187451922245430, -218.1519544391847489, 95.22527181742790958 ) ) ;
#5862 = ORIENTED_EDGE ( 'NONE', *, *, #2686, .T. ) ;
#5863 = PRODUCT_CONTEXT ( 'NONE', #106, 'mechanical' ) ;
#5864 = EDGE_CURVE ( 'NONE', #2680, #2858, #7289, .T. ) ;
#5865 = DIRECTION ( 'NONE',  ( -1.000000000000000000, 0.000000000000000000, -8.673617379884035472E-16 ) ) ;
#5866 = DIRECTION ( 'NONE',  ( 1.000000000000000000, 0.000000000000000000, 0.000000000000000000 ) ) ;
#5867 = CIRCLE ( 'NONE', #5496, 3.000000000000002665 ) ;
#5868 = ORIENTED_EDGE ( 'NONE', *, *, #6620, .T. ) ;
#5869 = DIRECTION ( 'NONE',  ( -0.4999999999999976130, 0.000000000000000000, -0.8660254037844399289 ) ) ;
#5870 = DIRECTION ( 'NONE',  ( 5.605193857299270773E-45, 0.000000000000000000, 1.000000000000000000 ) ) ;
#5871 = EDGE_CURVE ( 'NONE', #7205, #2384, #3656, .T. ) ;
#5872 = CARTESIAN_POINT ( 'NONE',  ( 19.77324663291341622, -218.0630240738404950, 77.42037680107310393 ) ) ;
#5873 = DIRECTION ( 'NONE',  ( -1.000000000000000000, 0.000000000000000000, 0.000000000000000000 ) ) ;
#5874 = LINE ( 'NONE', #5410, #2825 ) ;
#5875 = ORIENTED_EDGE ( 'NONE', *, *, #7105, .T. ) ;
#5876 = CARTESIAN_POINT ( 'NONE',  ( 0.000000000000000000, 0.000000000000000000, 0.000000000000000000 ) ) ;
#5877 = DIRECTION ( 'NONE',  ( 0.000000000000000000, 0.000000000000000000, -1.000000000000000000 ) ) ;
#5878 = DIRECTION ( 'NONE',  ( -0.4999999999999950595, -0.000000000000000000, -0.8660254037844414832 ) ) ;
#5879 = CARTESIAN_POINT ( 'NONE',  ( 188.9119595497369062, -5.725408222392992741, 18.47444250808088029 ) ) ;
#5880 = EDGE_CURVE ( 'NONE', #6005, #722, #290, .T. ) ;
#5881 = EDGE_CURVE ( 'NONE', #7091, #7026, #2263, .T. ) ;
#5882 = EDGE_LOOP ( 'NONE', ( #3551, #2855, #2918, #4053 ) ) ;
#5883 = ORIENTED_EDGE ( 'NONE', *, *, #7147, .T. ) ;
#5884 = DIRECTION ( 'NONE',  ( 0.000000000000000000, 0.000000000000000000, -1.000000000000000000 ) ) ;
#5885 = CARTESIAN_POINT ( 'NONE',  ( 192.1021416551216419, 6.000000000000000000, 18.00000000000001066 ) ) ;
#5886 = ORIENTED_EDGE ( 'NONE', *, *, #5968, .T. ) ;
#5887 = CARTESIAN_POINT ( 'NONE',  ( -70.16044999292957129, -220.0996966972331848, 78.34180846956243727 ) ) ;
#5888 = CYLINDRICAL_SURFACE ( 'NONE', #4765, 2.999999999999999112 ) ;
#5889 = EDGE_CURVE ( 'NONE', #917, #920, #3497, .T. ) ;
#5890 = CYLINDRICAL_SURFACE ( 'NONE', #1527, 3.000000000000000000 ) ;
#5891 = ORIENTED_EDGE ( 'NONE', *, *, #2725, .T. ) ;
#5892 = ORIENTED_EDGE ( 'NONE', *, *, #5871, .T. ) ;
#5893 = CARTESIAN_POINT ( 'NONE',  ( 0.000000000000000000, 0.000000000000000000, -39.99999999999997868 ) ) ;
#5894 = CARTESIAN_POINT ( 'NONE',  ( 17.83418965632456121, -223.7273137069674931, 96.20835808347007401 ) ) ;
#5895 = VERTEX_POINT ( 'NONE', #3574 ) ;
#5896 = LINE ( 'NONE', #6625, #4570 ) ;
#5897 = CARTESIAN_POINT ( 'NONE',  ( 1.387778780781445676E-14, 101.5000000000000000, 4.999999999999999112 ) ) ;
#5898 = VERTEX_POINT ( 'NONE', #5914 ) ;
#5899 = EDGE_CURVE ( 'NONE', #4244, #6501, #5084, .T. ) ;
#5900 = EDGE_CURVE ( 'NONE', #4443, #2926, #6925, .T. ) ;
#5901 = CARTESIAN_POINT ( 'NONE',  ( 217.0000000000000000, -56.99999999999999289, 3.000000000000000444 ) ) ;
#5902 = AXIS2_PLACEMENT_3D ( 'NONE', #5609, #6291, #1018 ) ;
#5903 = DIRECTION ( 'NONE',  ( 1.224646799147352714E-16, 1.000000000000000000, -6.864382715941954980E-61 ) ) ;
#5904 = CARTESIAN_POINT ( 'NONE',  ( 18.63742165201374945, -218.0630240738404666, 75.93507306776972143 ) ) ;
#5905 = CARTESIAN_POINT ( 'NONE',  ( 21.42066185573919412, -223.0630240738404666, 86.48599461439638958 ) ) ;
#5906 = CARTESIAN_POINT ( 'NONE',  ( 188.6380400399839061, 9.000000000000001776, 15.00000000000000888 ) ) ;
#5907 = AXIS2_PLACEMENT_3D ( 'NONE', #132, #663, #1933 ) ;
#5908 = ORIENTED_EDGE ( 'NONE', *, *, #4594, .T. ) ;
#5909 = ORIENTED_EDGE ( 'NONE', *, *, #3271, .T. ) ;
#5910 = CARTESIAN_POINT ( 'NONE',  ( 220.0000000000000000, 18.00000000000000000, 7.000000000000008882 ) ) ;
#5911 = DIRECTION ( 'NONE',  ( -1.000000000000000000, -0.000000000000000000, -0.000000000000000000 ) ) ;
#5912 = DIRECTION ( 'NONE',  ( 5.551115123125783935E-17, 0.7071067811865499042, 0.7071067811865451302 ) ) ;
#5913 = CARTESIAN_POINT ( 'NONE',  ( 24.99999999999999289, 86.00000000000001421, 4.999999999999992006 ) ) ;
#5914 = CARTESIAN_POINT ( 'NONE',  ( 209.9999999999999716, -6.000000000000000000, 41.00000000000002132 ) ) ;
#5915 = VECTOR ( 'NONE', #7536, 1000.000000000000000 ) ;
#5916 = DIRECTION ( 'NONE',  ( 1.000000000000000000, 1.853902270198408060E-44, 1.681558157189780485E-44 ) ) ;
#5917 =( BOUNDED_CURVE ( )  B_SPLINE_CURVE ( 3, ( #1589, #3877, #2675, #332 ),
 .UNSPECIFIED., .F., .T. ) 
 B_SPLINE_CURVE_WITH_KNOTS ( ( 4, 4 ),
 ( -1.776356839400250465E-15, 1.570796326794894782 ),
 .UNSPECIFIED. ) 
 CURVE ( )  GEOMETRIC_REPRESENTATION_ITEM ( )  RATIONAL_B_SPLINE_CURVE ( ( 1.000000000000000000, 0.8047378541243649375, 0.8047378541243649375, 1.000000000000000000 ) ) 
 REPRESENTATION_ITEM ( '' )  );
#5918 = ORIENTED_EDGE ( 'NONE', *, *, #5899, .T. ) ;
#5919 = ORIENTED_EDGE ( 'NONE', *, *, #1741, .T. ) ;
#5920 = EDGE_CURVE ( 'NONE', #131, #1634, #3491, .T. ) ;
#5921 = LINE ( 'NONE', #648, #457 ) ;
#5922 = AXIS2_PLACEMENT_3D ( 'NONE', #836, #231, #2570 ) ;
#5923 = CYLINDRICAL_SURFACE ( 'NONE', #7301, 3.000000000000000888 ) ;
#5924 = ORIENTED_EDGE ( 'NONE', *, *, #1396, .T. ) ;
#5925 = CARTESIAN_POINT ( 'NONE',  ( -60.77671317003689211, -224.6695236240148290, 73.71173840043843484 ) ) ;
#5926 = CARTESIAN_POINT ( 'NONE',  ( -21.49999999999999289, -67.16361968246712877, 40.16361968246722824 ) ) ;
#5927 = DIRECTION ( 'NONE',  ( 1.000000000000000000, 0.000000000000000000, 0.000000000000000000 ) ) ;
#5928 = ORIENTED_EDGE ( 'NONE', *, *, #1495, .T. ) ;
#5929 = VERTEX_POINT ( 'NONE', #7111 ) ;
#5930 =( BOUNDED_CURVE ( )  B_SPLINE_CURVE ( 3, ( #5050, #4986, #5019, #7470 ),
 .UNSPECIFIED., .F., .T. ) 
 B_SPLINE_CURVE_WITH_KNOTS ( ( 4, 4 ),
 ( 3.141592653589793116, 4.712388980384689674 ),
 .UNSPECIFIED. ) 
 CURVE ( )  GEOMETRIC_REPRESENTATION_ITEM ( )  RATIONAL_B_SPLINE_CURVE ( ( 1.000000000000000000, 0.8047378541243649375, 0.8047378541243649375, 1.000000000000000000 ) ) 
 REPRESENTATION_ITEM ( '' )  );
#5931 = EDGE_CURVE ( 'NONE', #238, #4710, #2503, .T. ) ;
#5932 = CARTESIAN_POINT ( 'NONE',  ( 220.0000000000000000, 3.000000000000000000, 35.00000000000000000 ) ) ;
#5933 = DIRECTION ( 'NONE',  ( 1.000000000000000000, 0.000000000000000000, 0.000000000000000000 ) ) ;
#5934 = VERTEX_POINT ( 'NONE', #4414 ) ;
#5935 = DIRECTION ( 'NONE',  ( 1.000000000000000000, 0.000000000000000000, 0.000000000000000000 ) ) ;
#5936 = LINE ( 'NONE', #2900, #2863 ) ;
#5937 = ORIENTED_EDGE ( 'NONE', *, *, #5624, .T. ) ;
#5938 = PLANE ( 'NONE',  #4889 ) ;
#5939 = DIRECTION ( 'NONE',  ( -1.000000000000000000, 5.551115123125783935E-17, -4.237045877651919561E-33 ) ) ;
#5940 = CIRCLE ( 'NONE', #2619, 8.500000000000007105 ) ;
#5941 =( NAMED_UNIT ( * ) SI_UNIT ( $, .STERADIAN. ) SOLID_ANGLE_UNIT ( ) );
#5942 = CARTESIAN_POINT ( 'NONE',  ( 21.45574242475734650, -218.0630240738404950, 84.84425821389238820 ) ) ;
#5943 = FACE_OUTER_BOUND ( 'NONE', #6803, .T. ) ;
#5944 = DIRECTION ( 'NONE',  ( -1.000000000000000000, 0.000000000000000000, 0.000000000000000000 ) ) ;
#5945 = EDGE_CURVE ( 'NONE', #3412, #5460, #6588, .T. ) ;
#5946 = PRODUCT_DEFINITION_CONTEXT ( 'detailed design', #2693, 'design' ) ;
#5947 = CIRCLE ( 'NONE', #6930, 14.00000000000000533 ) ;
#5948 = DIRECTION ( 'NONE',  ( 1.000000000000000000, 2.465190328815661892E-32, -9.244463733058732095E-33 ) ) ;
#5949 = DIRECTION ( 'NONE',  ( 0.000000000000000000, 8.881784197001252323E-16, -1.000000000000000000 ) ) ;
#5950 = CARTESIAN_POINT ( 'NONE',  ( 217.0000000000000000, -56.99999999999999289, 0.000000000000000000 ) ) ;
#5951 = FACE_OUTER_BOUND ( 'NONE', #5127, .T. ) ;
#5952 = DIRECTION ( 'NONE',  ( -0.8660254037844413721, 0.000000000000000000, 0.4999999999999950595 ) ) ;
#5953 = LINE ( 'NONE', #6499, #738 ) ;
#5954 = AXIS2_PLACEMENT_3D ( 'NONE', #1692, #2885, #574 ) ;
#5955 = EDGE_CURVE ( 'NONE', #5154, #1377, #2742, .T. ) ;
#5956 = VECTOR ( 'NONE', #4648, 1000.000000000000114 ) ;
#5957 = AXIS2_PLACEMENT_3D ( 'NONE', #3959, #3387, #525 ) ;
#5958 = ORIENTED_EDGE ( 'NONE', *, *, #7567, .T. ) ;
#5959 = EDGE_LOOP ( 'NONE', ( #6623, #5520, #5442, #1486 ) ) ;
#5960 = CIRCLE ( 'NONE', #3635, 3.000000000000000888 ) ;
#5961 = AXIS2_PLACEMENT_3D ( 'NONE', #6719, #791, #1444 ) ;
#5962 = CARTESIAN_POINT ( 'NONE',  ( 217.0000000000000000, 6.000000000000000000, 18.00000000000001066 ) ) ;
#5963 = FACE_OUTER_BOUND ( 'NONE', #218, .T. ) ;
#5964 = VERTEX_POINT ( 'NONE', #5638 ) ;
#5965 = CARTESIAN_POINT ( 'NONE',  ( -60.82928583850154780, -228.1620966263574246, 74.64757051591659831 ) ) ;
#5966 = ADVANCED_FACE ( 'NONE', ( #978 ), #2134, .F. ) ;
#5967 = CARTESIAN_POINT ( 'NONE',  ( -57.48968592151182833, -218.0630067422592617, 94.36623590530653871 ) ) ;
#5968 = EDGE_CURVE ( 'NONE', #529, #597, #6802, .T. ) ;
#5969 =( GEOMETRIC_REPRESENTATION_CONTEXT ( 3 ) GLOBAL_UNCERTAINTY_ASSIGNED_CONTEXT ( ( #2481 ) ) GLOBAL_UNIT_ASSIGNED_CONTEXT ( ( #2476, #1355, #2625 ) ) REPRESENTATION_CONTEXT ( 'NONE', 'WORKASPACE' ) );
#5970 = ORIENTED_EDGE ( 'NONE', *, *, #2161, .T. ) ;
#5971 = EDGE_LOOP ( 'NONE', ( #3619, #1358 ) ) ;
#5972 = DIRECTION ( 'NONE',  ( 4.622231866529368100E-33, -2.600005424922769496E-32, 1.000000000000000000 ) ) ;
#5973 = DIRECTION ( 'NONE',  ( 0.000000000000000000, 0.000000000000000000, -1.000000000000000000 ) ) ;
#5974 = ORIENTED_EDGE ( 'NONE', *, *, #2936, .F. ) ;
#5975 = DIRECTION ( 'NONE',  ( 0.000000000000000000, 0.000000000000000000, -1.000000000000000000 ) ) ;
#5976 = DIRECTION ( 'NONE',  ( -0.000000000000000000, 1.000000000000000000, 0.000000000000000000 ) ) ;
#5977 = EDGE_CURVE ( 'NONE', #4634, #2155, #6831, .T. ) ;
#5978 = ADVANCED_FACE ( 'NONE', ( #3914 ), #5179, .T. ) ;
#5979 = EDGE_LOOP ( 'NONE', ( #7248, #3397 ) ) ;
#5980 = VECTOR ( 'NONE', #5687, 1000.000000000000000 ) ;
#5981 = PRODUCT_DEFINITION ( 'UNKNOWN', '', #6089, #1794 ) ;
#5982 = CARTESIAN_POINT ( 'NONE',  ( 220.0000000000000000, 15.08392021690038121, 15.00000000000000888 ) ) ;
#5983 = CARTESIAN_POINT ( 'NONE',  ( 217.0000000000000000, 56.99999999999999289, 3.000000000000021760 ) ) ;
#5984 = CIRCLE ( 'NONE', #2175, 3.000000000000000000 ) ;
#5985 = CARTESIAN_POINT ( 'NONE',  ( 25.00000000000000000, 73.78679656440354506, 5.999999999999996447 ) ) ;
#5986 = CYLINDRICAL_SURFACE ( 'NONE', #1238, 3.000000000000000000 ) ;
#5987 = DIRECTION ( 'NONE',  ( 0.000000000000000000, -1.000000000000000000, -0.000000000000000000 ) ) ;
#5988 = EDGE_CURVE ( 'NONE', #6611, #3579, #2008, .T. ) ;
#5989 = AXIS2_PLACEMENT_3D ( 'NONE', #4872, #137, #7207 ) ;
#5990 = CARTESIAN_POINT ( 'NONE',  ( 0.000000000000000000, 0.000000000000000000, 48.99999999999999289 ) ) ;
#5991 = SURFACE_STYLE_FILL_AREA ( #3178 ) ;
#5992 = CARTESIAN_POINT ( 'NONE',  ( 49.62135916575378047, 25.53693568588315799, 12.86832014125687884 ) ) ;
#5993 = CARTESIAN_POINT ( 'NONE',  ( -21.50000000000000000, -215.0630240738403813, -2.498001805406602216E-13 ) ) ;
#5994 = DIRECTION ( 'NONE',  ( -1.000000000000000000, 0.000000000000000000, 0.000000000000000000 ) ) ;
#5995 = DIRECTION ( 'NONE',  ( 0.000000000000000000, 0.000000000000000000, -1.000000000000000000 ) ) ;
#5996 = CARTESIAN_POINT ( 'NONE',  ( 189.0752568151670800, -7.489143060488414605, 15.37864083427403195 ) ) ;
#5997 = ORIENTED_EDGE ( 'NONE', *, *, #1434, .T. ) ;
#5998 = ORIENTED_EDGE ( 'NONE', *, *, #3711, .F. ) ;
#5999 = ADVANCED_FACE ( 'NONE', ( #5608 ), #331, .F. ) ;
#6000 = CYLINDRICAL_SURFACE ( 'NONE', #5369, 2.999999999999999556 ) ;
#6001 = CARTESIAN_POINT ( 'NONE',  ( -21.50000000000000000, -105.5631177942458407, 67.24940929526130162 ) ) ;
#6002 = CARTESIAN_POINT ( 'NONE',  ( 12.50000000000001066, 12.50000000000001066, 0.000000000000000000 ) ) ;
#6003 = CARTESIAN_POINT ( 'NONE',  ( 47.78524365475726654, -25.70892696317056192, 12.89802653137118860 ) ) ;
#6004 = CARTESIAN_POINT ( 'NONE',  ( -59.85703050705383532, -218.0624546635179399, 93.03239386934940569 ) ) ;
#6005 = VERTEX_POINT ( 'NONE', #7445 ) ;
#6006 = ORIENTED_EDGE ( 'NONE', *, *, #1670, .T. ) ;
#6007 = ADVANCED_FACE ( 'NONE', ( #2099 ), #107, .T. ) ;
#6008 = CARTESIAN_POINT ( 'NONE',  ( 0.000000000000000000, 0.000000000000000000, -9.999999999999994671 ) ) ;
#6009 = CARTESIAN_POINT ( 'NONE',  ( 10.25365409304695952, -222.9757987891379400, 73.25790619872482523 ) ) ;
#6010 = ORIENTED_EDGE ( 'NONE', *, *, #7457, .T. ) ;
#6011 = FACE_OUTER_BOUND ( 'NONE', #127, .T. ) ;
#6012 = CARTESIAN_POINT ( 'NONE',  ( -32.50000000000002842, -49.37258300203047412, -15.99999999999998579 ) ) ;
#6013 = ORIENTED_EDGE ( 'NONE', *, *, #7097, .F. ) ;
#6014 = PLANE ( 'NONE',  #1816 ) ;
#6015 = EDGE_CURVE ( 'NONE', #5743, #4738, #4846, .T. ) ;
#6016 = CARTESIAN_POINT ( 'NONE',  ( 0.000000000000000000, 0.000000000000000000, 35.00000000000000000 ) ) ;
#6017 = CARTESIAN_POINT ( 'NONE',  ( -27.07790214619733860, -113.7796841263389069, 41.77968412633906325 ) ) ;
#6018 = DIRECTION ( 'NONE',  ( -5.868966822792461377E-17, 0.9848077530122080203, -0.1736481776669304422 ) ) ;
#6019 = CIRCLE ( 'NONE', #4964, 2.999999999999999112 ) ;
#6020 = SURFACE_SIDE_STYLE ('',( #1324 ) ) ;
#6021 = AXIS2_PLACEMENT_3D ( 'NONE', #2580, #736, #5480 ) ;
#6022 = UNCERTAINTY_MEASURE_WITH_UNIT (LENGTH_MEASURE( 1.000000000000000082E-05 ), #214, 'distance_accuracy_value', 'NONE');
#6023 = EDGE_LOOP ( 'NONE', ( #4279, #2283, #6048, #4314 ) ) ;
#6024 = AXIS2_PLACEMENT_3D ( 'NONE', #6338, #1675, #4606 ) ;
#6025 = CIRCLE ( 'NONE', #985, 15.99999999999997691 ) ;
#6026 = DIRECTION ( 'NONE',  ( 1.000000000000000000, 2.465190328815661892E-32, -9.244463733058732095E-33 ) ) ;
#6027 = EDGE_CURVE ( 'NONE', #6493, #5278, #659, .T. ) ;
#6028 =( LENGTH_UNIT ( ) NAMED_UNIT ( * ) SI_UNIT ( .MILLI., .METRE. ) );
#6029 = CARTESIAN_POINT ( 'NONE',  ( 217.0000000000000000, 9.000000000000001776, 15.00000000000000888 ) ) ;
#6030 = DIRECTION ( 'NONE',  ( 0.000000000000000000, -1.000000000000000000, 0.000000000000000000 ) ) ;
#6031 = CARTESIAN_POINT ( 'NONE',  ( -63.60636663337245267, -223.0630240873432797, 80.31129794962551216 ) ) ;
#6032 = DIRECTION ( 'NONE',  ( 1.000000000000000000, 2.465190328815661892E-32, -9.244463733058732095E-33 ) ) ;
#6033 = ADVANCED_FACE ( 'NONE', ( #2368 ), #517, .T. ) ;
#6034 = AXIS2_PLACEMENT_3D ( 'NONE', #1891, #3091, #3597 ) ;
#6035 = ORIENTED_EDGE ( 'NONE', *, *, #5840, .F. ) ;
#6036 = ORIENTED_EDGE ( 'NONE', *, *, #1851, .F. ) ;
#6037 = AXIS2_PLACEMENT_3D ( 'NONE', #2080, #3164, #5622 ) ;
#6038 = DIRECTION ( 'NONE',  ( -0.000000000000000000, -0.000000000000000000, 1.000000000000000000 ) ) ;
#6039 = DIRECTION ( 'NONE',  ( 0.000000000000000000, 0.000000000000000000, -1.000000000000000000 ) ) ;
#6040 = CARTESIAN_POINT ( 'NONE',  ( -60.80066350777958206, -226.2606222968802854, 74.13807200489549132 ) ) ;
#6041 = DIRECTION ( 'NONE',  ( 0.000000000000000000, 0.000000000000000000, -1.000000000000000000 ) ) ;
#6042 = DIRECTION ( 'NONE',  ( -2.465190328815661892E-32, -1.000000000000000000, -1.193489751472043281E-15 ) ) ;
#6043 = ADVANCED_FACE ( 'NONE', ( #7060 ), #1750, .F. ) ;
#6044 = ORIENTED_EDGE ( 'NONE', *, *, #4094, .T. ) ;
#6045 = ORIENTED_EDGE ( 'NONE', *, *, #3314, .T. ) ;
#6046 = CARTESIAN_POINT ( 'NONE',  ( 12.50000000000000355, 101.5000000000000000, 4.999999999999999112 ) ) ;
#6047 = CARTESIAN_POINT ( 'NONE',  ( 17.81252276423129999, -227.0484711946332936, 74.34917548081020300 ) ) ;
#6048 = ORIENTED_EDGE ( 'NONE', *, *, #2603, .T. ) ;
#6049 = FACE_OUTER_BOUND ( 'NONE', #241, .T. ) ;
#6050 = CARTESIAN_POINT ( 'NONE',  ( -10.49999999999997513, 16.00000000000006750, 32.26953873476009704 ) ) ;
#6051 = AXIS2_PLACEMENT_3D ( 'NONE', #4112, #2339, #1331 ) ;
#6052 = ORIENTED_EDGE ( 'NONE', *, *, #2139, .F. ) ;
#6053 = CARTESIAN_POINT ( 'NONE',  ( -64.50000000000000000, -104.1739323729103575, 75.12787131935894536 ) ) ;
#6054 = CARTESIAN_POINT ( 'NONE',  ( 40.00000000000000000, -4.163336342344337027E-14, 1.387778780781445676E-14 ) ) ;
#6055 = ORIENTED_EDGE ( 'NONE', *, *, #3544, .T. ) ;
#6056 = DIRECTION ( 'NONE',  ( 4.622231866529368100E-33, -2.600005424922769496E-32, 1.000000000000000000 ) ) ;
#6057 = DIRECTION ( 'NONE',  ( 1.000000000000000000, 0.000000000000000000, 0.000000000000000000 ) ) ;
#6058 = CARTESIAN_POINT ( 'NONE',  ( 217.0000000000000000, 9.000000000000001776, 12.00000000000000711 ) ) ;
#6059 = ADVANCED_FACE ( 'NONE', ( #2940 ), #6452, .F. ) ;
#6060 = EDGE_CURVE ( 'NONE', #3729, #4322, #6955, .T. ) ;
#6061 = CIRCLE ( 'NONE', #7166, 6.000000000000000888 ) ;
#6062 = DIRECTION ( 'NONE',  ( -1.000000000000000000, 0.000000000000000000, 0.000000000000000000 ) ) ;
#6063 = DIRECTION ( 'NONE',  ( 0.000000000000000000, 0.000000000000000000, -1.000000000000000000 ) ) ;
#6064 = DIRECTION ( 'NONE',  ( 1.000000000000000000, -5.551115123125783935E-17, 4.237045877651919561E-33 ) ) ;
#6065 = CARTESIAN_POINT ( 'NONE',  ( -56.68590668195482607, -223.0634275682792236, 73.83207632951022958 ) ) ;
#6066 = DIRECTION ( 'NONE',  ( 8.673617379884035472E-16, 0.000000000000000000, -1.000000000000000000 ) ) ;
#6067 = VECTOR ( 'NONE', #2790, 1000.000000000000000 ) ;
#6068 = ADVANCED_FACE ( 'NONE', ( #2797 ), #2869, .T. ) ;
#6069 = VERTEX_POINT ( 'NONE', #1100 ) ;
#6070 = ORIENTED_EDGE ( 'NONE', *, *, #5424, .F. ) ;
#6071 = CARTESIAN_POINT ( 'NONE',  ( 50.51471862576143224, -28.78532416918554304, 10.00000000000000711 ) ) ;
#6072 = VECTOR ( 'NONE', #6649, 1000.000000000000114 ) ;
#6073 = DIRECTION ( 'NONE',  ( 0.000000000000000000, 0.000000000000000000, -1.000000000000000000 ) ) ;
#6074 = AXIS2_PLACEMENT_3D ( 'NONE', #2682, #3342, #7408 ) ;
#6075 = VECTOR ( 'NONE', #3095, 1000.000000000000000 ) ;
#6076 = CARTESIAN_POINT ( 'NONE',  ( 6.500000000000002665, 101.5000000000000000, -1.214306433183764966E-14 ) ) ;
#6077 = CARTESIAN_POINT ( 'NONE',  ( 220.0000000000000000, -15.08392021690038121, 12.00000000000000711 ) ) ;
#6078 = CARTESIAN_POINT ( 'NONE',  ( -63.70849213729819382, -218.0630240738405519, 87.94705950315832865 ) ) ;
#6079 = ORIENTED_EDGE ( 'NONE', *, *, #3575, .T. ) ;
#6080 = MECHANICAL_DESIGN_GEOMETRIC_PRESENTATION_REPRESENTATION (  '', ( #5588 ), #4485 ) ;
#6081 = VECTOR ( 'NONE', #5117, 1000.000000000000000 ) ;
#6082 = EDGE_LOOP ( 'NONE', ( #5886, #6149, #5578, #3191 ) ) ;
#6083 = CARTESIAN_POINT ( 'NONE',  ( -26.50000000000003197, -102.6862915010150346, 30.68629150101517666 ) ) ;
#6084 = CARTESIAN_POINT ( 'NONE',  ( 10.06880420804609422, -218.8824061789517259, 72.16108495452192528 ) ) ;
#6085 = ORIENTED_EDGE ( 'NONE', *, *, #1949, .F. ) ;
#6086 = ITEM_DEFINED_TRANSFORMATION ( 'NONE', 'NONE', #4499,  #1914 ) ;
#6087 = AXIS2_PLACEMENT_3D ( 'NONE', #773, #6661, #3124 ) ;
#6088 = CARTESIAN_POINT ( 'NONE',  ( 26.00000000000000000, 0.000000000000000000, 0.000000000000000000 ) ) ;
#6089 = PRODUCT_DEFINITION_FORMATION_WITH_SPECIFIED_SOURCE ( 'ANY', '', #3210, .NOT_KNOWN. ) ;
#6090 = CARTESIAN_POINT ( 'NONE',  ( 21.50000000000000000, -49.37258300203045280, 5.999999999999972466 ) ) ;
#6091 = ORIENTED_EDGE ( 'NONE', *, *, #1376, .F. ) ;
#6092 = FACE_BOUND ( 'NONE', #6095, .T. ) ;
#6093 = EDGE_CURVE ( 'NONE', #429, #1140, #3859, .T. ) ;
#6094 = DIRECTION ( 'NONE',  ( 0.000000000000000000, 1.000000000000000000, -1.445602896647337931E-16 ) ) ;
#6095 = EDGE_LOOP ( 'NONE', ( #2311, #3782 ) ) ;
#6096 = EDGE_CURVE ( 'NONE', #1895, #4729, #5826, .T. ) ;
#6097 = FACE_OUTER_BOUND ( 'NONE', #4418, .T. ) ;
#6098 = DIRECTION ( 'NONE',  ( 1.000000000000000000, 0.000000000000000000, 0.000000000000000000 ) ) ;
#6099 = CIRCLE ( 'NONE', #444, 6.000000000000000000 ) ;
#6100 = PLANE ( 'NONE',  #6107 ) ;
#6101 = EDGE_CURVE ( 'NONE', #5513, #2163, #1147, .T. ) ;
#6102 = DIRECTION ( 'NONE',  ( 1.000000000000000000, 0.000000000000000000, 0.000000000000000000 ) ) ;
#6103 = LINE ( 'NONE', #1403, #553 ) ;
#6104 = CARTESIAN_POINT ( 'NONE',  ( -61.17229153618341542, -223.0630242530635883, 76.63199592159693907 ) ) ;
#6105 = ORIENTED_EDGE ( 'NONE', *, *, #4772, .T. ) ;
#6106 = DIRECTION ( 'NONE',  ( 4.622231866529368100E-33, -2.600005424922769496E-32, 1.000000000000000000 ) ) ;
#6107 = AXIS2_PLACEMENT_3D ( 'NONE', #6134, #6209, #860 ) ;
#6108 = ORIENTED_EDGE ( 'NONE', *, *, #2571, .F. ) ;
#6109 = ORIENTED_EDGE ( 'NONE', *, *, #1081, .F. ) ;
#6110 = LINE ( 'NONE', #6580, #5242 ) ;
#6111 = VECTOR ( 'NONE', #2364, 1000.000000000000000 ) ;
#6112 = CARTESIAN_POINT ( 'NONE',  ( 201.3397459621555470, 3.000000000000000000, 39.99999999999999289 ) ) ;
#6113 = EDGE_CURVE ( 'NONE', #4244, #1140, #5802, .T. ) ;
#6114 = CARTESIAN_POINT ( 'NONE',  ( -26.50000000000003197, -7.347880794884112834E-16, -6.000000000000001776 ) ) ;
#6115 = CARTESIAN_POINT ( 'NONE',  ( 4.000000000000000000, 1.224646799147350101E-15, -9.999999999999998224 ) ) ;
#6116 = ORIENTED_EDGE ( 'NONE', *, *, #4877, .T. ) ;
#6117 = ORIENTED_EDGE ( 'NONE', *, *, #6607, .T. ) ;
#6118 = CARTESIAN_POINT ( 'NONE',  ( 2.775557561562891351E-14, 36.67766952966363903, 4.535533905932717325 ) ) ;
#6119 = DIRECTION ( 'NONE',  ( -0.7071067811865497932, 8.659560562354715921E-17, -0.7071067811865452413 ) ) ;
#6120 = EDGE_CURVE ( 'NONE', #4312, #5684, #7415, .T. ) ;
#6121 = ORIENTED_EDGE ( 'NONE', *, *, #7175, .F. ) ;
#6122 = DIRECTION ( 'NONE',  ( -1.000000000000000000, 0.000000000000000000, -7.663350976776343357E-46 ) ) ;
#6123 = FACE_OUTER_BOUND ( 'NONE', #6655, .T. ) ;
#6124 = ORIENTED_EDGE ( 'NONE', *, *, #4411, .F. ) ;
#6125 = CARTESIAN_POINT ( 'NONE',  ( 47.00000000000000000, 30.03170604878415162, 10.00000000000000888 ) ) ;
#6126 = CARTESIAN_POINT ( 'NONE',  ( 47.00000000000000000, 27.04312195450891565, 12.73853277175702559 ) ) ;
#6127 = ORIENTED_EDGE ( 'NONE', *, *, #1870, .T. ) ;
#6128 =( BOUNDED_CURVE ( )  B_SPLINE_CURVE ( 3, ( #5340, #3573, #4774, #7110 ),
 .UNSPECIFIED., .F., .T. ) 
 B_SPLINE_CURVE_WITH_KNOTS ( ( 4, 4 ),
 ( 0.6981317007977386746, 1.570796326794897446 ),
 .UNSPECIFIED. ) 
 CURVE ( )  GEOMETRIC_REPRESENTATION_ITEM ( )  RATIONAL_B_SPLINE_CURVE ( ( 1.000000000000000000, 0.9375385246911008830, 0.9375385246911008830, 1.000000000000000000 ) ) 
 REPRESENTATION_ITEM ( '' )  );
#6129 = DIRECTION ( 'NONE',  ( -7.623657272262513435E-17, 0.7071067811865465735, -0.7071067811865484609 ) ) ;
#6130 = DIRECTION ( 'NONE',  ( 0.000000000000000000, -1.000000000000000000, -1.221245327087672392E-15 ) ) ;
#6131 = CARTESIAN_POINT ( 'NONE',  ( 21.50000000000000000, -49.37258300203045280, -2.775557561562891351E-14 ) ) ;
#6132 = EDGE_CURVE ( 'NONE', #2795, #7224, #780, .T. ) ;
#6133 = ORIENTED_EDGE ( 'NONE', *, *, #6203, .F. ) ;
#6134 = CARTESIAN_POINT ( 'NONE',  ( 24.99999999999999289, 86.00000000000001421, 4.999999999999992006 ) ) ;
#6135 = DIRECTION ( 'NONE',  ( 0.000000000000000000, 0.000000000000000000, 1.000000000000000000 ) ) ;
#6136 = CARTESIAN_POINT ( 'NONE',  ( -64.17143802327697699, -223.0612697797253361, 87.56774190916064526 ) ) ;
#6137 = CARTESIAN_POINT ( 'NONE',  ( 188.1331788443806374, -8.454652614717035775, 15.00000000000001066 ) ) ;
#6138 = CARTESIAN_POINT ( 'NONE',  ( -10.49999999999996803, -49.37258300203045280, -2.775557561562891351E-14 ) ) ;
#6139 = ORIENTED_EDGE ( 'NONE', *, *, #7186, .F. ) ;
#6140 = ORIENTED_EDGE ( 'NONE', *, *, #571, .F. ) ;
#6141 = DIRECTION ( 'NONE',  ( -0.000000000000000000, 1.000000000000000000, 0.000000000000000000 ) ) ;
#6142 = DIRECTION ( 'NONE',  ( 1.000000000000000000, 2.624548829666596736E-30, -9.231085635203017994E-31 ) ) ;
#6143 = CARTESIAN_POINT ( 'NONE',  ( 3.469446951953614189E-14, 80.85786437626907741, 8.071067811865438202 ) ) ;
#6144 = UNCERTAINTY_MEASURE_WITH_UNIT (LENGTH_MEASURE( 1.000000000000000082E-05 ), #6028, 'distance_accuracy_value', 'NONE');
#6145 = ORIENTED_EDGE ( 'NONE', *, *, #2515, .T. ) ;
#6146 = EDGE_CURVE ( 'NONE', #233, #7468, #1596, .T. ) ;
#6147 = VERTEX_POINT ( 'NONE', #3303 ) ;
#6148 = DIRECTION ( 'NONE',  ( 5.254869241218065572E-46, -0.7071067811865465735, 0.7071067811865485719 ) ) ;
#6149 = ORIENTED_EDGE ( 'NONE', *, *, #4810, .F. ) ;
#6150 = CIRCLE ( 'NONE', #4819, 7.999999999999986677 ) ;
#6151 = DIRECTION ( 'NONE',  ( 5.605193857299270773E-45, 0.000000000000000000, 1.000000000000000000 ) ) ;
#6152 = DIRECTION ( 'NONE',  ( 1.000000000000000000, 0.000000000000000000, 0.000000000000000000 ) ) ;
#6153 = ORIENTED_EDGE ( 'NONE', *, *, #3681, .T. ) ;
#6154 = AXIS2_PLACEMENT_3D ( 'NONE', #254, #4488, #3331 ) ;
#6155 = EDGE_CURVE ( 'NONE', #3340, #4643, #4364, .T. ) ;
#6156 = EDGE_CURVE ( 'NONE', #3448, #162, #373, .T. ) ;
#6157 = DIRECTION ( 'NONE',  ( 5.605193857299270773E-45, 0.000000000000000000, 1.000000000000000000 ) ) ;
#6158 = DIRECTION ( 'NONE',  ( 1.000000000000000000, -0.000000000000000000, -0.000000000000000000 ) ) ;
#6159 = DIRECTION ( 'NONE',  ( 1.000000000000000000, 0.000000000000000000, 0.000000000000000000 ) ) ;
#6160 = VERTEX_POINT ( 'NONE', #7373 ) ;
#6161 = VECTOR ( 'NONE', #802, 1000.000000000000000 ) ;
#6162 = CARTESIAN_POINT ( 'NONE',  ( 23.99999999999999289, 0.000000000000000000, 1.345246525751824388E-43 ) ) ;
#6163 = CARTESIAN_POINT ( 'NONE',  ( 185.0000000000000000, 39.99999999999999289, 0.000000000000000000 ) ) ;
#6164 = FILL_AREA_STYLE_COLOUR ( '', #6756 ) ;
#6165 = EDGE_LOOP ( 'NONE', ( #876, #5011, #5167, #4468, #3516, #69, #1734 ) ) ;
#6166 = EDGE_LOOP ( 'NONE', ( #3170, #884, #2910, #7261 ) ) ;
#6167 = CARTESIAN_POINT ( 'NONE',  ( 4.000000000000000000, 0.000000000000000000, 0.000000000000000000 ) ) ;
#6168 = DIRECTION ( 'NONE',  ( 1.000000000000000000, 0.000000000000000000, 0.000000000000000000 ) ) ;
#6169 = CARTESIAN_POINT ( 'NONE',  ( -32.50000000000002842, -49.37258300203047412, 6.000000000000000888 ) ) ;
#6170 = CARTESIAN_POINT ( 'NONE',  ( -60.48402471930579338, -223.0632605723740767, 75.98548927210011072 ) ) ;
#6171 = ORIENTED_EDGE ( 'NONE', *, *, #748, .T. ) ;
#6172 = DIRECTION ( 'NONE',  ( -1.000000000000000000, 0.000000000000000000, -7.663350976776343357E-46 ) ) ;
#6173 = EDGE_LOOP ( 'NONE', ( #6667, #5315, #4365, #405 ) ) ;
#6174 = VERTEX_POINT ( 'NONE', #4455 ) ;
#6175 = CARTESIAN_POINT ( 'NONE',  ( -21.50000000000000000, -120.9522879036832848, 45.92078884797942351 ) ) ;
#6176 = EDGE_CURVE ( 'NONE', #1843, #3503, #5070, .T. ) ;
#6177 = DIRECTION ( 'NONE',  ( -0.000000000000000000, -0.000000000000000000, 1.000000000000000000 ) ) ;
#6178 = CARTESIAN_POINT ( 'NONE',  ( -26.49999999999999645, -99.90626354475344328, 72.90626354475362803 ) ) ;
#6179 = VECTOR ( 'NONE', #6369, 1000.000000000000000 ) ;
#6180 = AXIS2_PLACEMENT_3D ( 'NONE', #2933, #5284, #51 ) ;
#6181 = ORIENTED_EDGE ( 'NONE', *, *, #4117, .T. ) ;
#6182 = ORIENTED_EDGE ( 'NONE', *, *, #5302, .F. ) ;
#6183 = AXIS2_PLACEMENT_3D ( 'NONE', #964, #4436, #7387 ) ;
#6184 = EDGE_CURVE ( 'NONE', #2192, #597, #1641, .T. ) ;
#6185 = DIRECTION ( 'NONE',  ( 0.6444004775717538935, 0.5407162030609466985, -0.5407162030609481418 ) ) ;
#6186 = ORIENTED_EDGE ( 'NONE', *, *, #1583, .F. ) ;
#6187 = DIRECTION ( 'NONE',  ( 1.000000000000000000, 0.000000000000000000, 0.000000000000000000 ) ) ;
#6188 = DIRECTION ( 'NONE',  ( 0.000000000000000000, 0.000000000000000000, -1.000000000000000000 ) ) ;
#6189 = CIRCLE ( 'NONE', #300, 3.000000000000000000 ) ;
#6190 = CIRCLE ( 'NONE', #1898, 15.99999999999998934 ) ;
#6191 = CIRCLE ( 'NONE', #1649, 22.00000000000000355 ) ;
#6192 = ORIENTED_EDGE ( 'NONE', *, *, #4675, .T. ) ;
#6193 = DIRECTION ( 'NONE',  ( 9.231085635203016242E-31, 0.000000000000000000, -1.000000000000000000 ) ) ;
#6194 = AXIS2_PLACEMENT_3D ( 'NONE', #3897, #5659, #2728 ) ;
#6195 = CARTESIAN_POINT ( 'NONE',  ( 50.68728032240937864, 28.82511565990200708, 10.00000000000000888 ) ) ;
#6196 = DIRECTION ( 'NONE',  ( 0.000000000000000000, 0.000000000000000000, 1.000000000000000000 ) ) ;
#6197 = CIRCLE ( 'NONE', #5961, 3.000000000000006217 ) ;
#6198 = VERTEX_POINT ( 'NONE', #3384 ) ;
#6199 = DIRECTION ( 'NONE',  ( 0.000000000000000000, 0.000000000000000000, 1.000000000000000000 ) ) ;
#6200 = CARTESIAN_POINT ( 'NONE',  ( -53.25562355766778921, -218.1519544391847774, 95.22527181742790958 ) ) ;
#6201 = EDGE_CURVE ( 'NONE', #6764, #5705, #4236, .T. ) ;
#6202 = FACE_OUTER_BOUND ( 'NONE', #6551, .T. ) ;
#6203 = EDGE_CURVE ( 'NONE', #1231, #5033, #6806, .T. ) ;
#6204 = CARTESIAN_POINT ( 'NONE',  ( 50.00000000000001421, -15.08392021690038121, 12.00000000000000711 ) ) ;
#6205 = ORIENTED_EDGE ( 'NONE', *, *, #6864, .F. ) ;
#6206 = VERTEX_POINT ( 'NONE', #2755 ) ;
#6207 =( GEOMETRIC_REPRESENTATION_CONTEXT ( 3 ) GLOBAL_UNCERTAINTY_ASSIGNED_CONTEXT ( ( #3490 ) ) GLOBAL_UNIT_ASSIGNED_CONTEXT ( ( #743, #820, #7283 ) ) REPRESENTATION_CONTEXT ( 'NONE', 'WORKASPACE' ) );
#6208 = ORIENTED_EDGE ( 'NONE', *, *, #3005, .T. ) ;
#6209 = DIRECTION ( 'NONE',  ( -4.237045877651920929E-33, -2.600005424922769496E-32, 1.000000000000000000 ) ) ;
#6210 = DIRECTION ( 'NONE',  ( 0.000000000000000000, 0.000000000000000000, -1.000000000000000000 ) ) ;
#6211 = CARTESIAN_POINT ( 'NONE',  ( 53.00000000000000711, 24.00878702352406435, 13.00000000000000888 ) ) ;
#6212 = CARTESIAN_POINT ( 'NONE',  ( -58.17782861558893615, -223.0629528839427564, 95.01857375712019405 ) ) ;
#6213 = EDGE_CURVE ( 'NONE', #1381, #3944, #3500, .T. ) ;
#6214 = DIRECTION ( 'NONE',  ( -0.000000000000000000, -0.000000000000000000, 1.000000000000000000 ) ) ;
#6215 = CARTESIAN_POINT ( 'NONE',  ( -16.16037543966235646, -114.3720785834762665, 42.37207858347650102 ) ) ;
#6216 = DIRECTION ( 'NONE',  ( 1.000000000000000000, 2.465190328815661892E-32, -9.244463733058732095E-33 ) ) ;
#6217 = ORIENTED_EDGE ( 'NONE', *, *, #2739, .F. ) ;
#6218 = ORIENTED_EDGE ( 'NONE', *, *, #2603, .F. ) ;
#6219 = CARTESIAN_POINT ( 'NONE',  ( -21.50000000000000000, -215.0630240738404950, 94.68061005248806339 ) ) ;
#6220 = DIRECTION ( 'NONE',  ( -3.503246160812044233E-46, 0.9659258262890683122, -0.2588190451025208505 ) ) ;
#6221 = CARTESIAN_POINT ( 'NONE',  ( 25.00000000000000711, 77.32233047033632545, 4.535533905932710219 ) ) ;
#6222 = DIRECTION ( 'NONE',  ( -2.465190328815662439E-32, -1.000000000000000000, -5.551115123125783935E-17 ) ) ;
#6223 = CIRCLE ( 'NONE', #1186, 8.000000000000007105 ) ;
#6224 = VERTEX_POINT ( 'NONE', #5728 ) ;
#6225 = ADVANCED_FACE ( 'NONE', ( #453 ), #4575, .F. ) ;
#6226 = ORIENTED_EDGE ( 'NONE', *, *, #7514, .T. ) ;
#6227 = ADVANCED_FACE ( 'NONE', ( #2450 ), #112, .F. ) ;
#6228 = CIRCLE ( 'NONE', #2051, 9.999999999999996447 ) ;
#6229 = DIRECTION ( 'NONE',  ( -1.000000000000000000, -2.624548829666596736E-30, 9.231085635203017994E-31 ) ) ;
#6230 = ORIENTED_EDGE ( 'NONE', *, *, #3348, .F. ) ;
#6231 = CARTESIAN_POINT ( 'NONE',  ( 220.0000000000000000, 6.000000000000000000, 35.00000000000000000 ) ) ;
#6232 = CARTESIAN_POINT ( 'NONE',  ( 40.00000000000000000, -4.163336342344337027E-14, 1.387778780781445676E-14 ) ) ;
#6233 = APPLICATION_CONTEXT ( 'automotive_design' ) ;
#6234 = ORIENTED_EDGE ( 'NONE', *, *, #6723, .T. ) ;
#6235 = ADVANCED_FACE ( 'NONE', ( #1215 ), #3610, .T. ) ;
#6236 = CARTESIAN_POINT ( 'NONE',  ( 7.318533788671489235E-30, 1.102182119232615150E-15, 7.999999999999989342 ) ) ;
#6237 = CARTESIAN_POINT ( 'NONE',  ( 0.000000000000000000, 0.000000000000000000, 0.000000000000000000 ) ) ;
#6238 = ORIENTED_EDGE ( 'NONE', *, *, #5177, .T. ) ;
#6239 = DIRECTION ( 'NONE',  ( -3.703017452606044190E-17, 1.000000000000000000, -2.976165145832578406E-18 ) ) ;
#6240 = CARTESIAN_POINT ( 'NONE',  ( -60.66255603274095165, -212.1022451272887110, 94.15854484029743787 ) ) ;
#6241 = DIRECTION ( 'NONE',  ( 0.000000000000000000, 0.000000000000000000, -1.000000000000000000 ) ) ;
#6242 = DIRECTION ( 'NONE',  ( 0.000000000000000000, 0.000000000000000000, 1.000000000000000000 ) ) ;
#6243 = EDGE_LOOP ( 'NONE', ( #2194, #1820 ) ) ;
#6244 = EDGE_LOOP ( 'NONE', ( #4278, #931, #3245, #986, #563, #6192 ) ) ;
#6245 = ADVANCED_FACE ( 'NONE', ( #7597 ), #3032, .T. ) ;
#6246 = LINE ( 'NONE', #3257, #2909 ) ;
#6247 =( NAMED_UNIT ( * ) SI_UNIT ( $, .STERADIAN. ) SOLID_ANGLE_UNIT ( ) );
#6248 = CARTESIAN_POINT ( 'NONE',  ( 189.2277783884485132, 5.808582712248391289, 19.02145678267364559 ) ) ;
#6249 = DIRECTION ( 'NONE',  ( 1.000000000000000000, 2.624548829666596736E-30, -9.231085635203017994E-31 ) ) ;
#6250 = FACE_OUTER_BOUND ( 'NONE', #4574, .T. ) ;
#6251 = DIRECTION ( 'NONE',  ( -0.000000000000000000, 1.000000000000000000, 0.000000000000000000 ) ) ;
#6252 = CARTESIAN_POINT ( 'NONE',  ( -29.50000000000000000, -223.0630240738404950, 96.09122589815579829 ) ) ;
#6253 = EDGE_LOOP ( 'NONE', ( #2343, #5017, #5241, #2143 ) ) ;
#6254 = EDGE_CURVE ( 'NONE', #6268, #640, #2752, .T. ) ;
#6255 = VERTEX_POINT ( 'NONE', #4655 ) ;
#6256 = DIRECTION ( 'NONE',  ( 0.000000000000000000, 0.000000000000000000, -1.000000000000000000 ) ) ;
#6257 = CARTESIAN_POINT ( 'NONE',  ( -16.49999999999996803, 16.00000000000012079, -15.99999999999995914 ) ) ;
#6258 = DIRECTION ( 'NONE',  ( 0.000000000000000000, 0.000000000000000000, -1.000000000000000000 ) ) ;
#6259 = PLANE ( 'NONE',  #4983 ) ;
#6260 = DIRECTION ( 'NONE',  ( -1.000000000000000000, 5.551115123125783935E-17, -4.237045877651919561E-33 ) ) ;
#6261 = AXIS2_PLACEMENT_3D ( 'NONE', #823, #7325, #1904 ) ;
#6262 = VERTEX_POINT ( 'NONE', #5225 ) ;
#6263 = ORIENTED_EDGE ( 'NONE', *, *, #2678, .F. ) ;
#6264 = MANIFOLD_SOLID_BREP ( 'Fillet1', #3812 ) ;
#6265 = CLOSED_SHELL ( 'NONE', ( #5999, #3150, #2860, #3900, #5978, #1242, #2818, #3806, #1395, #1299, #6227, #5500, #5966, #4061, #4754, #2924, #4285, #5746, #4671, #804, #4840, #6899, #2375, #6987, #4402, #2113, #4706, #5386, #6245, #740 ) ) ;
#6266 = VECTOR ( 'NONE', #4958, 1000.000000000000000 ) ;
#6267 = CARTESIAN_POINT ( 'NONE',  ( 209.9999999999999716, -6.000000000000000000, 35.00000000000000000 ) ) ;
#6268 = VERTEX_POINT ( 'NONE', #523 ) ;
#6269 = EDGE_CURVE ( 'NONE', #3365, #1652, #1658, .T. ) ;
#6270 = DIRECTION ( 'NONE',  ( 5.605193857299270773E-45, 0.000000000000000000, 1.000000000000000000 ) ) ;
#6271 = LINE ( 'NONE', #5742, #2402 ) ;
#6272 = CIRCLE ( 'NONE', #11, 2.999999999999999112 ) ;
#6273 = VERTEX_POINT ( 'NONE', #1832 ) ;
#6274 = AXIS2_PLACEMENT_3D ( 'NONE', #7347, #1533, #3817 ) ;
#6275 = CARTESIAN_POINT ( 'NONE',  ( 53.00000000000000000, 24.00878702352406435, 10.00000000000000888 ) ) ;
#6276 = DIRECTION ( 'NONE',  ( 0.000000000000000000, 1.000000000000000000, 3.304235192336776498E-16 ) ) ;
#6277 = MANIFOLD_SOLID_BREP ( 'Chamfer1', #2090 ) ;
#6278 = ORIENTED_EDGE ( 'NONE', *, *, #5632, .T. ) ;
#6279 = CARTESIAN_POINT ( 'NONE',  ( 218.7908117647228039, -11.00000000000001243, 79.99586816227022723 ) ) ;
#6280 = CARTESIAN_POINT ( 'NONE',  ( -70.00607124224620748, -224.5869008243856797, 90.77423662209318422 ) ) ;
#6281 = CARTESIAN_POINT ( 'NONE',  ( -30.49999999999998579, -218.0630240738404950, 95.20959099461346398 ) ) ;
#6282 = CARTESIAN_POINT ( 'NONE',  ( 43.50000000000001421, -39.99999999999999289, 10.00000000000000355 ) ) ;
#6283 = ORIENTED_EDGE ( 'NONE', *, *, #2945, .T. ) ;
#6284 = ORIENTED_EDGE ( 'NONE', *, *, #7545, .F. ) ;
#6285 = FACE_OUTER_BOUND ( 'NONE', #1097, .T. ) ;
#6286 = CONICAL_SURFACE ( 'NONE', #5682, 8.000000000000003553, 0.7853981633974447263 ) ;
#6287 = CARTESIAN_POINT ( 'NONE',  ( 200.0000000000000000, 11.00000000000000711, 8.660254037844383745 ) ) ;
#6288 = DIRECTION ( 'NONE',  ( 0.000000000000000000, 0.000000000000000000, 1.000000000000000000 ) ) ;
#6289 = EDGE_CURVE ( 'NONE', #5696, #5020, #1715, .T. ) ;
#6290 = DIRECTION ( 'NONE',  ( 1.000000000000000000, 0.000000000000000000, 0.000000000000000000 ) ) ;
#6291 = DIRECTION ( 'NONE',  ( -0.000000000000000000, -0.000000000000000000, 1.000000000000000000 ) ) ;
#6292 = CARTESIAN_POINT ( 'NONE',  ( 50.00000000000000000, -22.78166690339260825, 13.00000000000000711 ) ) ;
#6293 = EDGE_CURVE ( 'NONE', #452, #2583, #5214, .T. ) ;
#6294 = CARTESIAN_POINT ( 'NONE',  ( -53.75100615578827501, -218.0630240738404950, 71.94153218116485959 ) ) ;
#6295 = AXIS2_PLACEMENT_3D ( 'NONE', #4891, #4458, #1485 ) ;
#6296 = EDGE_LOOP ( 'NONE', ( #3786, #3366, #1191, #5069 ) ) ;
#6297 = ORIENTED_EDGE ( 'NONE', *, *, #4043, .T. ) ;
#6298 = CARTESIAN_POINT ( 'NONE',  ( -26.50000000000000355, -120.9522879036833558, 45.92078884797942351 ) ) ;
#6299 = CARTESIAN_POINT ( 'NONE',  ( -53.25365409304696840, -222.9757987891380253, 73.25790619872483944 ) ) ;
#6300 = DIRECTION ( 'NONE',  ( -0.000000000000000000, 0.000000000000000000, 1.000000000000000000 ) ) ;
#6301 = DIRECTION ( 'NONE',  ( 0.000000000000000000, -0.000000000000000000, -1.000000000000000000 ) ) ;
#6302 = CARTESIAN_POINT ( 'NONE',  ( 220.0000000000000000, -60.00000000000000000, 7.000000000000000888 ) ) ;
#6303 = ADVANCED_FACE ( 'NONE', ( #253 ), #6931, .T. ) ;
#6304 = EDGE_CURVE ( 'NONE', #1997, #3892, #2389, .T. ) ;
#6305 = PRODUCT_RELATED_PRODUCT_CATEGORY ( 'part', '', ( #2239 ) ) ;
#6306 = ORIENTED_EDGE ( 'NONE', *, *, #4878, .T. ) ;
#6307 = ORIENTED_EDGE ( 'NONE', *, *, #2677, .F. ) ;
#6308 = MANIFOLD_SOLID_BREP ( 'Cut-Extrude2', #737 ) ;
#6309 = AXIS2_PLACEMENT_3D ( 'NONE', #4597, #2126, #1087 ) ;
#6310 = DIRECTION ( 'NONE',  ( 0.000000000000000000, 0.000000000000000000, -1.000000000000000000 ) ) ;
#6311 = AXIS2_PLACEMENT_3D ( 'NONE', #6950, #1674, #6375 ) ;
#6312 = ORIENTED_EDGE ( 'NONE', *, *, #197, .F. ) ;
#6313 = CARTESIAN_POINT ( 'NONE',  ( -26.50000000000000000, -69.36092951174981636, 42.36092951174991583 ) ) ;
#6314 = CARTESIAN_POINT ( 'NONE',  ( -17.99999999999999645, 2.204364238465234244E-15, -39.99999999999997868 ) ) ;
#6315 = ORIENTED_EDGE ( 'NONE', *, *, #430, .T. ) ;
#6316 = COLOUR_RGB ( '',0.7921568627450980005, 0.8196078431372548767, 0.9333333333333333481 ) ;
#6317 = CARTESIAN_POINT ( 'NONE',  ( 4.000000000000003553, 0.000000000000000000, 10.00000000000001243 ) ) ;
#6318 = DIRECTION ( 'NONE',  ( 0.000000000000000000, 0.000000000000000000, -1.000000000000000000 ) ) ;
#6319 = ORIENTED_EDGE ( 'NONE', *, *, #1325, .T. ) ;
#6320 = CARTESIAN_POINT ( 'NONE',  ( 209.9999999999998295, -15.99999999999928590, 34.99999999999987210 ) ) ;
#6321 = CIRCLE ( 'NONE', #794, 8.000000000000007105 ) ;
#6322 = FACE_OUTER_BOUND ( 'NONE', #5200, .T. ) ;
#6323 = AXIS2_PLACEMENT_3D ( 'NONE', #1284, #5444, #776 ) ;
#6324 = DIRECTION ( 'NONE',  ( -1.000000000000000000, -1.853902270198408060E-44, -1.681558157189780485E-44 ) ) ;
#6325 = AXIS2_PLACEMENT_3D ( 'NONE', #5627, #2122, #6318 ) ;
#6326 = CARTESIAN_POINT ( 'NONE',  ( 12.50000000000001066, 12.50000000000001066, 4.999999999999995559 ) ) ;
#6327 = ORIENTED_EDGE ( 'NONE', *, *, #7155, .F. ) ;
#6328 = EDGE_LOOP ( 'NONE', ( #4474, #4207 ) ) ;
#6329 = AXIS2_PLACEMENT_3D ( 'NONE', #301, #4390, #3734 ) ;
#6330 = ADVANCED_FACE ( 'NONE', ( #4335 ), #182, .T. ) ;
#6331 = CIRCLE ( 'NONE', #3008, 8.500000000000007105 ) ;
#6332 = CIRCLE ( 'NONE', #189, 3.000000000000004885 ) ;
#6333 = EDGE_CURVE ( 'NONE', #5437, #2475, #291, .T. ) ;
#6334 = CARTESIAN_POINT ( 'NONE',  ( 4.000000000000000000, -2.624548829666593232E-30, 9.999999999999998224 ) ) ;
#6335 = SURFACE_STYLE_FILL_AREA ( #1624 ) ;
#6336 = FACE_OUTER_BOUND ( 'NONE', #2342, .T. ) ;
#6337 = CARTESIAN_POINT ( 'NONE',  ( 12.50000000000001066, 12.50000000000001066, -1.214306433183764966E-14 ) ) ;
#6338 = CARTESIAN_POINT ( 'NONE',  ( -32.50000000000002842, 6.938893903907228378E-15, 0.000000000000000000 ) ) ;
#6339 = DIRECTION ( 'NONE',  ( 0.000000000000000000, 0.000000000000000000, -1.000000000000000000 ) ) ;
#6341 = CARTESIAN_POINT ( 'NONE',  ( -61.15478436381093275, -218.0630249522653514, 75.41002070443643390 ) ) ;
#6340 =( GEOMETRIC_REPRESENTATION_CONTEXT ( 3 ) GLOBAL_UNCERTAINTY_ASSIGNED_CONTEXT ( ( #7104 ) ) GLOBAL_UNIT_ASSIGNED_CONTEXT ( ( #1246, #5289, #2298 ) ) REPRESENTATION_CONTEXT ( 'NONE', 'WORKASPACE' ) );
#6342 = ORIENTED_EDGE ( 'NONE', *, *, #4139, .T. ) ;
#6343 = ADVANCED_FACE ( 'NONE', ( #4881 ), #1894, .T. ) ;
#6344 = ORIENTED_EDGE ( 'NONE', *, *, #6685, .F. ) ;
#6345 = DIRECTION ( 'NONE',  ( 7.318533788671501715E-33, 1.945189243831109580E-32, -1.000000000000000000 ) ) ;
#6346 = DIRECTION ( 'NONE',  ( 4.622231866529368100E-33, -2.600005424922769496E-32, 1.000000000000000000 ) ) ;
#6347 = CARTESIAN_POINT ( 'NONE',  ( 201.3397459621555754, 3.000000000000000000, 39.99999999999997868 ) ) ;
#6348 = VECTOR ( 'NONE', #5501, 1000.000000000000000 ) ;
#6349 = EDGE_LOOP ( 'NONE', ( #2253, #4331, #4760, #4417 ) ) ;
#6350 = ORIENTED_EDGE ( 'NONE', *, *, #1905, .T. ) ;
#6351 = MANIFOLD_SOLID_BREP ( 'Fillet2', #1968 ) ;
#6352 = EDGE_CURVE ( 'NONE', #2768, #3264, #5101, .T. ) ;
#6353 = LINE ( 'NONE', #2312, #6724 ) ;
#6354 = AXIS2_PLACEMENT_3D ( 'NONE', #2527, #180, #7217 ) ;
#6355 = CARTESIAN_POINT ( 'NONE',  ( -13.35769912250762204, 16.00000000000006750, 38.39789427971190605 ) ) ;
#6356 = ORIENTED_EDGE ( 'NONE', *, *, #4688, .F. ) ;
#6357 = PRODUCT_DEFINITION_SHAPE ( 'NONE', 'NONE',  #1414 ) ;
#6358 = CARTESIAN_POINT ( 'NONE',  ( 53.00000000000000000, -22.78166690339260825, 10.00000000000000888 ) ) ;
#6359 = DIRECTION ( 'NONE',  ( 5.605193857299270773E-45, 0.000000000000000000, 1.000000000000000000 ) ) ;
#6360 = ORIENTED_EDGE ( 'NONE', *, *, #3776, .T. ) ;
#6361 = AXIS2_PLACEMENT_3D ( 'NONE', #5305, #2997, #3399 ) ;
#6362 = ORIENTED_EDGE ( 'NONE', *, *, #3767, .F. ) ;
#6363 = EDGE_CURVE ( 'NONE', #3579, #6611, #4611, .T. ) ;
#6364 = CARTESIAN_POINT ( 'NONE',  ( 10.10706597980996335, -219.7296907405071238, 72.38811416855006087 ) ) ;
#6365 = CARTESIAN_POINT ( 'NONE',  ( 27.00607124224622169, -224.5869008243855944, 90.77423662209318422 ) ) ;
#6366 = VERTEX_POINT ( 'NONE', #1014 ) ;
#6367 = CIRCLE ( 'NONE', #3051, 15.99999999999997335 ) ;
#6368 = CYLINDRICAL_SURFACE ( 'NONE', #5537, 2.999999999999999112 ) ;
#6369 = DIRECTION ( 'NONE',  ( 1.000000000000000000, 2.465190328815661892E-32, -9.244463733058732095E-33 ) ) ;
#6370 = EDGE_LOOP ( 'NONE', ( #4837, #611, #5857, #7106 ) ) ;
#6371 = VERTEX_POINT ( 'NONE', #3258 ) ;
#6372 = DIRECTION ( 'NONE',  ( 0.000000000000000000, 0.000000000000000000, -1.000000000000000000 ) ) ;
#6373 = DIRECTION ( 'NONE',  ( -1.000000000000000000, -1.725633230170963324E-31, 1.078147950931789387E-16 ) ) ;
#6374 = CARTESIAN_POINT ( 'NONE',  ( 189.5040654437683258, 6.000000000000000000, 19.50000000000000355 ) ) ;
#6375 = DIRECTION ( 'NONE',  ( 0.000000000000000000, 0.000000000000000000, 1.000000000000000000 ) ) ;
#6376 = CARTESIAN_POINT ( 'NONE',  ( 18.87504319907951356, -223.0630240738404666, 92.12888099325203939 ) ) ;
#6377 = DIRECTION ( 'NONE',  ( 1.000000000000000000, -5.551115123125783935E-17, 4.237045877651919561E-33 ) ) ;
#6378 = EDGE_CURVE ( 'NONE', #162, #1669, #3330, .T. ) ;
#6379 = CARTESIAN_POINT ( 'NONE',  ( -57.83326664796290117, -218.0630925741273813, 73.02699328150956148 ) ) ;
#6380 = ORIENTED_EDGE ( 'NONE', *, *, #7337, .T. ) ;
#6381 = DIRECTION ( 'NONE',  ( -0.000000000000000000, 1.000000000000000000, 1.836970198721029934E-16 ) ) ;
#6382 = CARTESIAN_POINT ( 'NONE',  ( 25.00000000000000711, 40.21320343559642652, 0.9999999999999956701 ) ) ;
#6383 = PLANE ( 'NONE',  #1900 ) ;
#6384 = CARTESIAN_POINT ( 'NONE',  ( 188.0000000000000000, -10.62218397927710356, -7.000000000000017764 ) ) ;
#6385 = PLANE ( 'NONE',  #7151 ) ;
#6386 = ORIENTED_EDGE ( 'NONE', *, *, #7186, .T. ) ;
#6387 = ORIENTED_EDGE ( 'NONE', *, *, #4232, .T. ) ;
#6388 = MANIFOLD_SOLID_BREP ( 'Cut-Extrude1', #134 ) ;
#6389 = CYLINDRICAL_SURFACE ( 'NONE', #3424, 5.999999999999999112 ) ;
#6390 = CARTESIAN_POINT ( 'NONE',  ( 2.775557561562891351E-14, 28.00000000000002487, 4.999999999999995559 ) ) ;
#6391 = ORIENTED_EDGE ( 'NONE', *, *, #1870, .F. ) ;
#6392 = AXIS2_PLACEMENT_3D ( 'NONE', #249, #4910, #7246 ) ;
#6393 = FACE_OUTER_BOUND ( 'NONE', #7584, .T. ) ;
#6394 = LINE ( 'NONE', #39, #1166 ) ;
#6395 = EDGE_CURVE ( 'NONE', #316, #1796, #2132, .T. ) ;
#6396 = ORIENTED_EDGE ( 'NONE', *, *, #5811, .F. ) ;
#6397 = AXIS2_PLACEMENT_3D ( 'NONE', #6138, #1986, #2531 ) ;
#6398 = PLANE ( 'NONE',  #905 ) ;
#6399 = CARTESIAN_POINT ( 'NONE',  ( 27.19709702122541017, -216.0025558445558431, 89.06679694989070128 ) ) ;
#6400 = ORIENTED_EDGE ( 'NONE', *, *, #5138, .T. ) ;
#6401 = CONTEXT_DEPENDENT_SHAPE_REPRESENTATION ( #3739, #5331 ) ;
#6402 = CIRCLE ( 'NONE', #2222, 10.00000000000000355 ) ;
#6403 = CARTESIAN_POINT ( 'NONE',  ( 3.000000000000000000, -28.78532416918554304, 7.000000000000006217 ) ) ;
#6404 = LINE ( 'NONE', #4794, #3971 ) ;
#6405 = EDGE_CURVE ( 'NONE', #4443, #4747, #5606, .T. ) ;
#6406 = ORIENTED_EDGE ( 'NONE', *, *, #7381, .F. ) ;
#6407 = AXIS2_PLACEMENT_3D ( 'NONE', #2691, #6701, #4975 ) ;
#6408 = PLANE ( 'NONE',  #3540 ) ;
#6409 = CARTESIAN_POINT ( 'NONE',  ( -18.84314575050759544, 16.00000000000003908, 36.34314575050770202 ) ) ;
#6410 = DIRECTION ( 'NONE',  ( 5.551115123125785167E-17, -0.7071067811865451302, 0.7071067811865499042 ) ) ;
#6411 = CARTESIAN_POINT ( 'NONE',  ( 15.03306249438985631, -218.0630240738404950, 73.12099198157908120 ) ) ;
#6412 = CARTESIAN_POINT ( 'NONE',  ( 4.000000000000003553, 1.224646799147353059E-15, -9.999999999999984013 ) ) ;
#6413 = FACE_OUTER_BOUND ( 'NONE', #5120, .T. ) ;
#6414 = MANIFOLD_SOLID_BREP ( 'Chamfer1', #3451 ) ;
#6415 = UNCERTAINTY_MEASURE_WITH_UNIT (LENGTH_MEASURE( 1.000000000000000082E-05 ), #1708, 'distance_accuracy_value', 'NONE');
#6416 = EDGE_LOOP ( 'NONE', ( #2587, #4536, #2325, #7424 ) ) ;
#6417 = VERTEX_POINT ( 'NONE', #1585 ) ;
#6418 = SURFACE_STYLE_FILL_AREA ( #4072 ) ;
#6419 = CARTESIAN_POINT ( 'NONE',  ( 0.000000000000000000, 0.000000000000000000, 0.000000000000000000 ) ) ;
#6420 = DIRECTION ( 'NONE',  ( 1.000000000000000000, 0.000000000000000000, 0.000000000000000000 ) ) ;
#6421 = CARTESIAN_POINT ( 'NONE',  ( 188.0259799560787997, 8.302416934599655463, 15.00000000000000711 ) ) ;
#6422 = CARTESIAN_POINT ( 'NONE',  ( -15.48397095257170974, -67.18204818810112045, 40.18204818810124124 ) ) ;
#6423 = AXIS2_PLACEMENT_3D ( 'NONE', #7243, #1902, #7284 ) ;
#6424 = VERTEX_POINT ( 'NONE', #6287 ) ;
#6425 = ORIENTED_EDGE ( 'NONE', *, *, #7419, .F. ) ;
#6426 = ADVANCED_FACE ( 'NONE', ( #898 ), #3372, .F. ) ;
#6427 = DIRECTION ( 'NONE',  ( -1.000000000000000000, 5.551115123125783935E-17, -4.237045877651919561E-33 ) ) ;
#6428 = CARTESIAN_POINT ( 'NONE',  ( 4.000000000000000000, 0.000000000000000000, 0.000000000000000000 ) ) ;
#6429 = VERTEX_POINT ( 'NONE', #5026 ) ;
#6430 = CARTESIAN_POINT ( 'NONE',  ( 25.00000000000002842, 33.14213562373094391, 8.071067811865434649 ) ) ;
#6431 = CARTESIAN_POINT ( 'NONE',  ( 21.50000000000000000, -39.68629150101519087, 15.99999999999998579 ) ) ;
#6432 = ORIENTED_EDGE ( 'NONE', *, *, #5138, .F. ) ;
#6433 = VERTEX_POINT ( 'NONE', #6789 ) ;
#6434 = AXIS2_PLACEMENT_3D ( 'NONE', #1740, #1125, #2324 ) ;
#6435 = EDGE_CURVE ( 'NONE', #2976, #6541, #6454, .T. ) ;
#6436 = CARTESIAN_POINT ( 'NONE',  ( 2.775557561562891351E-14, 28.00000000000002487, -1.734723475976807094E-15 ) ) ;
#6437 = CARTESIAN_POINT ( 'NONE',  ( 10.06880420804609422, -213.9340789708228669, 94.48154657108734966 ) ) ;
#6438 = ORIENTED_EDGE ( 'NONE', *, *, #5745, .T. ) ;
#6439 = ITEM_DEFINED_TRANSFORMATION ( 'NONE', 'NONE', #5234,  #1914 ) ;
#6440 = CARTESIAN_POINT ( 'NONE',  ( -26.49999999999999645, -104.1739323729103859, 75.12787131935894536 ) ) ;
#6441 = DIRECTION ( 'NONE',  ( 1.000000000000000000, -5.551115123125783935E-17, 4.237045877651919561E-33 ) ) ;
#6442 = VECTOR ( 'NONE', #2240, 1000.000000000000000 ) ;
#6443 = AXIS2_PLACEMENT_3D ( 'NONE', #2265, #3885, #4038 ) ;
#6444 = ORIENTED_EDGE ( 'NONE', *, *, #3403, .T. ) ;
#6445 = CARTESIAN_POINT ( 'NONE',  ( 50.00000000000000000, 17.97033316447826579, 12.83599132585211322 ) ) ;
#6446 = VECTOR ( 'NONE', #3088, 1000.000000000000000 ) ;
#6447 = AXIS2_PLACEMENT_3D ( 'NONE', #750, #1474, #7254 ) ;
#6448 = EDGE_CURVE ( 'NONE', #1494, #2116, #1283, .T. ) ;
#6449 = DIRECTION ( 'NONE',  ( -2.465190328815661892E-32, -1.000000000000000000, -1.193489751472043281E-15 ) ) ;
#6450 = EDGE_CURVE ( 'NONE', #7540, #2908, #2366, .T. ) ;
#6451 = CARTESIAN_POINT ( 'NONE',  ( 217.0000000000000000, -6.000000000000000000, 18.00000000000001066 ) ) ;
#6452 = PLANE ( 'NONE',  #897 ) ;
#6453 = CARTESIAN_POINT ( 'NONE',  ( 21.50932527815889728, -223.0630240738404666, 85.38297702798109867 ) ) ;
#6454 = CIRCLE ( 'NONE', #6575, 3.000000000000002665 ) ;
#6455 = AXIS2_PLACEMENT_3D ( 'NONE', #826, #1946, #4998 ) ;
#6456 = ORIENTED_EDGE ( 'NONE', *, *, #2405, .F. ) ;
#6457 = ORIENTED_EDGE ( 'NONE', *, *, #449, .T. ) ;
#6458 = EDGE_CURVE ( 'NONE', #1663, #1964, #3389, .T. ) ;
#6459 = DIRECTION ( 'NONE',  ( -1.681558157189779489E-44, 0.000000000000000000, -1.000000000000000000 ) ) ;
#6460 = DIRECTION ( 'NONE',  ( -1.000000000000000000, -0.000000000000000000, -0.000000000000000000 ) ) ;
#6461 = DIRECTION ( 'NONE',  ( 0.000000000000000000, 0.000000000000000000, 1.000000000000000000 ) ) ;
#6462 = CIRCLE ( 'NONE', #1906, 25.00000000000000000 ) ;
#6463 = CARTESIAN_POINT ( 'NONE',  ( -10.49999999999996803, 0.000000000000000000, 5.999999999999999112 ) ) ;
#6464 = ORIENTED_EDGE ( 'NONE', *, *, #1082, .F. ) ;
#6465 = ORIENTED_EDGE ( 'NONE', *, *, #5818, .F. ) ;
#6466 = CARTESIAN_POINT ( 'NONE',  ( 3.000000000000000000, 56.99999999999999289, 7.000000000000022204 ) ) ;
#6467 = DIRECTION ( 'NONE',  ( 0.000000000000000000, 0.000000000000000000, -1.000000000000000000 ) ) ;
#6468 = ORIENTED_EDGE ( 'NONE', *, *, #4051, .T. ) ;
#6469 = CARTESIAN_POINT ( 'NONE',  ( -70.14230383934500423, -218.4648600334252535, 89.55655311265203977 ) ) ;
#6470 = CARTESIAN_POINT ( 'NONE',  ( 47.78553976602403708, -28.78532416918281456, 10.00000000000000533 ) ) ;
#6471 = DIRECTION ( 'NONE',  ( -1.000000000000000000, 0.000000000000000000, 0.000000000000000000 ) ) ;
#6472 = EDGE_CURVE ( 'NONE', #2971, #1164, #1170, .T. ) ;
#6473 = ORIENTED_EDGE ( 'NONE', *, *, #492, .F. ) ;
#6474 = ORIENTED_EDGE ( 'NONE', *, *, #6435, .F. ) ;
#6475 = SHAPE_REPRESENTATION ( 'link', ( #1914 ), #7073 ) ;
#6476 = CARTESIAN_POINT ( 'NONE',  ( 50.00000000000000000, -17.91234734164656928, 13.00000000000000888 ) ) ;
#6477 = DIRECTION ( 'NONE',  ( 5.551115123125783935E-17, 1.000000000000000000, -2.214819436045321778E-32 ) ) ;
#6478 = ORIENTED_EDGE ( 'NONE', *, *, #4035, .F. ) ;
#6479 = CONTEXT_DEPENDENT_SHAPE_REPRESENTATION ( #2944, #5761 ) ;
#6480 = DIRECTION ( 'NONE',  ( 0.000000000000000000, 0.000000000000000000, -1.000000000000000000 ) ) ;
#6481 = DIRECTION ( 'NONE',  ( 1.000000000000000000, 0.000000000000000000, 0.000000000000000000 ) ) ;
#6482 = CIRCLE ( 'NONE', #3773, 6.000000000000000000 ) ;
#6483 = ORIENTED_EDGE ( 'NONE', *, *, #4361, .T. ) ;
#6484 = VECTOR ( 'NONE', #2235, 1000.000000000000000 ) ;
#6485 = LINE ( 'NONE', #1203, #5502 ) ;
#6486 = DIRECTION ( 'NONE',  ( 0.000000000000000000, 0.000000000000000000, -1.000000000000000000 ) ) ;
#6487 = ORIENTED_EDGE ( 'NONE', *, *, #1002, .T. ) ;
#6488 = CARTESIAN_POINT ( 'NONE',  ( 17.77546999798919103, -218.0630240738405519, 92.26857489675208512 ) ) ;
#6489 = CARTESIAN_POINT ( 'NONE',  ( 17.86619911493601620, -223.0630240738404666, 93.22347854821404667 ) ) ;
#6490 = CARTESIAN_POINT ( 'NONE',  ( 4.000000000000000000, 7.347880794883831802E-16, -6.000000000000000888 ) ) ;
#6491 = PRODUCT_DEFINITION_CONTEXT ( 'detailed design', #7027, 'design' ) ;
#6492 = EDGE_CURVE ( 'NONE', #2796, #316, #3871, .T. ) ;
#6493 = VERTEX_POINT ( 'NONE', #4682 ) ;
#6494 = DIRECTION ( 'NONE',  ( 1.000000000000000000, 0.000000000000000000, 0.000000000000000000 ) ) ;
#6495 = FILL_AREA_STYLE_COLOUR ( '', #2014 ) ;
#6496 = DIRECTION ( 'NONE',  ( 1.000000000000000000, 0.000000000000000000, -0.000000000000000000 ) ) ;
#6497 = CARTESIAN_POINT ( 'NONE',  ( 40.00000000000000000, -4.163336342344337027E-14, 1.387778780781445676E-14 ) ) ;
#6498 = CARTESIAN_POINT ( 'NONE',  ( 50.00000000000000000, 18.00000000000000000, 15.00000000000000888 ) ) ;
#6499 = CARTESIAN_POINT ( 'NONE',  ( 170.0000000000000000, 11.00000000000000533, -8.660254037844387298 ) ) ;
#6500 = EDGE_CURVE ( 'NONE', #7571, #5934, #3754, .T. ) ;
#6501 = VERTEX_POINT ( 'NONE', #5371 ) ;
#6502 = EDGE_LOOP ( 'NONE', ( #6920, #6988, #144, #4911 ) ) ;
#6503 = ADVANCED_FACE ( 'NONE', ( #4722 ), #5288, .F. ) ;
#6504 = FACE_OUTER_BOUND ( 'NONE', #3010, .T. ) ;
#6505 = DIRECTION ( 'NONE',  ( 1.000000000000000000, 0.000000000000000000, 0.000000000000000000 ) ) ;
#6506 = EDGE_LOOP ( 'NONE', ( #3950, #6140, #3286, #482 ) ) ;
#6507 = CARTESIAN_POINT ( 'NONE',  ( -60.83418965632457542, -228.4878731603066910, 74.73486207509363055 ) ) ;
#6508 = CARTESIAN_POINT ( 'NONE',  ( -16.49999999999996447, -39.68629150101520509, 23.99999999999999289 ) ) ;
#6509 = DIRECTION ( 'NONE',  ( -4.930380657631323236E-32, -0.9848077530122080203, 0.1736481776669304422 ) ) ;
#6510 = ORIENTED_EDGE ( 'NONE', *, *, #756, .T. ) ;
#6511 = ORIENTED_EDGE ( 'NONE', *, *, #5955, .F. ) ;
#6512 = EDGE_CURVE ( 'NONE', #1269, #1529, #7546, .T. ) ;
#6513 = CARTESIAN_POINT ( 'NONE',  ( 50.00000000000000000, -24.54223912878477165, 12.93866904445501120 ) ) ;
#6514 = CARTESIAN_POINT ( 'NONE',  ( 10.40199052334513041, -221.4565245236570377, 95.80795668296244116 ) ) ;
#6515 = EDGE_LOOP ( 'NONE', ( #7322, #6618, #6826, #6964, #6010, #7494, #2688, #4388 ) ) ;
#6516 = PRODUCT_CONTEXT ( 'NONE', #6233, 'mechanical' ) ;
#6517 = CYLINDRICAL_SURFACE ( 'NONE', #2832, 4.000000000000003553 ) ;
#6518 = AXIS2_PLACEMENT_3D ( 'NONE', #4103, #6057, #5329 ) ;
#6519 = AXIS2_PLACEMENT_3D ( 'NONE', #6634, #3173, #1357 ) ;
#6520 = EDGE_LOOP ( 'NONE', ( #235, #5390, #1810, #2057 ) ) ;
#6521 = FACE_OUTER_BOUND ( 'NONE', #2843, .T. ) ;
#6522 = EDGE_CURVE ( 'NONE', #4660, #959, #2760, .T. ) ;
#6523 = AXIS2_PLACEMENT_3D ( 'NONE', #4793, #4758, #5935 ) ;
#6524 = FACE_OUTER_BOUND ( 'NONE', #3093, .T. ) ;
#6525 = EDGE_LOOP ( 'NONE', ( #4581, #6774 ) ) ;
#6526 = CARTESIAN_POINT ( 'NONE',  ( 18.04970750630426579, -218.0630240738405519, 92.00715684020322271 ) ) ;
#6527 = DIRECTION ( 'NONE',  ( -0.000000000000000000, 1.000000000000000000, 3.304235192336776498E-16 ) ) ;
#6528 = CARTESIAN_POINT ( 'NONE',  ( 209.9999999999999716, 3.000000000000000000, 35.00000000000000000 ) ) ;
#6529 = PRODUCT ( 'left arm', 'left arm', '', ( #586 ) ) ;
#6530 = VECTOR ( 'NONE', #7314, 1000.000000000000000 ) ;
#6531 = CARTESIAN_POINT ( 'NONE',  ( 3.000000000000002665, 56.99999999999999289, 3.000000000000021760 ) ) ;
#6532 = EDGE_CURVE ( 'NONE', #4282, #4634, #6190, .T. ) ;
#6533 = FILL_AREA_STYLE_COLOUR ( '', #3379 ) ;
#6534 = DIRECTION ( 'NONE',  ( 0.000000000000000000, -1.000000000000000000, -1.221245327087672392E-15 ) ) ;
#6535 = DIRECTION ( 'NONE',  ( -1.000000000000000000, 0.000000000000000000, -7.663350976776343357E-46 ) ) ;
#6536 = LINE ( 'NONE', #5382, #3371 ) ;
#6537 = TOROIDAL_SURFACE ( 'NONE', #6037, 6.000000000000000000, 3.000000000000000000 ) ;
#6538 = EDGE_CURVE ( 'NONE', #6429, #7551, #2029, .T. ) ;
#6539 = LINE ( 'NONE', #4807, #5655 ) ;
#6540 = AXIS2_PLACEMENT_3D ( 'NONE', #6419, #1137, #3495 ) ;
#6541 = VERTEX_POINT ( 'NONE', #4764 ) ;
#6542 = VERTEX_POINT ( 'NONE', #4029 ) ;
#6543 = CARTESIAN_POINT ( 'NONE',  ( 53.00000000000000711, -22.78166690339260825, 10.00000000000000711 ) ) ;
#6544 = DIRECTION ( 'NONE',  ( 0.000000000000000000, 0.000000000000000000, 1.000000000000000000 ) ) ;
#6545 = ADVANCED_FACE ( 'NONE', ( #555 ), #67, .T. ) ;
#6546 = EDGE_CURVE ( 'NONE', #4861, #2624, #4368, .T. ) ;
#6547 = ORIENTED_EDGE ( 'NONE', *, *, #5077, .T. ) ;
#6548 = CARTESIAN_POINT ( 'NONE',  ( -69.99871551551807158, -227.2977332969690849, 80.10323607719463723 ) ) ;
#6549 = CARTESIAN_POINT ( 'NONE',  ( -23.84314575050760965, -63.65685424949226956, 36.65685424949239035 ) ) ;
#6550 = FACE_OUTER_BOUND ( 'NONE', #6506, .T. ) ;
#6551 = EDGE_LOOP ( 'NONE', ( #666, #1177, #89, #48 ) ) ;
#6552 = EDGE_LOOP ( 'NONE', ( #4133, #4081, #6315, #3021, #7450, #7096, #7130, #4993, #6145, #3090 ) ) ;
#6553 = CARTESIAN_POINT ( 'NONE',  ( -10.49999999999996803, -49.37258300203045280, -6.000000000000029310 ) ) ;
#6554 = CARTESIAN_POINT ( 'NONE',  ( 17.72636667137882682, -221.3248423084426975, 72.81553374298033532 ) ) ;
#6555 = ORIENTED_EDGE ( 'NONE', *, *, #5438, .F. ) ;
#6556 = CARTESIAN_POINT ( 'NONE',  ( 2.000000000000001776, 0.000000000000000000, 0.000000000000000000 ) ) ;
#6557 = DIRECTION ( 'NONE',  ( 0.000000000000000000, 0.000000000000000000, 1.000000000000000000 ) ) ;
#6558 = EDGE_LOOP ( 'NONE', ( #4026, #5173, #5924, #4969 ) ) ;
#6559 = DIRECTION ( 'NONE',  ( -1.000000000000000000, 5.551115123125783935E-17, -4.237045877651919561E-33 ) ) ;
#6560 = DIRECTION ( 'NONE',  ( 5.605193857299270773E-45, 0.000000000000000000, 1.000000000000000000 ) ) ;
#6561 = CARTESIAN_POINT ( 'NONE',  ( 17.35616244728660718, -218.0630240738405519, 92.64882813447223953 ) ) ;
#6562 = FACE_OUTER_BOUND ( 'NONE', #1420, .T. ) ;
#6563 = LINE ( 'NONE', #4104, #7245 ) ;
#6564 = ADVANCED_FACE ( 'NONE', ( #6524 ), #3602, .F. ) ;
#6565 = VECTOR ( 'NONE', #2546, 1000.000000000000114 ) ;
#6566=STYLED_ITEM('',(#7638),#6308);
#6567 = FACE_OUTER_BOUND ( 'NONE', #2879, .T. ) ;
#6568 =( LENGTH_UNIT ( ) NAMED_UNIT ( * ) SI_UNIT ( .MILLI., .METRE. ) );
#6569 = CARTESIAN_POINT ( 'NONE',  ( 49.39900052591443114, 25.87352760396088058, 12.83931617239071166 ) ) ;
#6570 = DIRECTION ( 'NONE',  ( 1.000000000000000000, 0.000000000000000000, 0.000000000000000000 ) ) ;
#6571 = CARTESIAN_POINT ( 'NONE',  ( 21.50000000000000000, -223.0630240738404382, 73.28127814332047762 ) ) ;
#6572 = CARTESIAN_POINT ( 'NONE',  ( -21.51784377693468642, -113.7796841263389069, 41.77968412633906325 ) ) ;
#6573 = CARTESIAN_POINT ( 'NONE',  ( 186.1301251221888720, -7.429512690641201011, 13.65616394131904343 ) ) ;
#6574 = VECTOR ( 'NONE', #1568, 1000.000000000000000 ) ;
#6575 = AXIS2_PLACEMENT_3D ( 'NONE', #3874, #1747, #5325 ) ;
#6576 = AXIS2_PLACEMENT_3D ( 'NONE', #7233, #3160, #4934 ) ;
#6577 = VERTEX_POINT ( 'NONE', #4141 ) ;
#6578 = ORIENTED_EDGE ( 'NONE', *, *, #757, .T. ) ;
#6579 = VECTOR ( 'NONE', #7592, 1000.000000000000000 ) ;
#6580 = CARTESIAN_POINT ( 'NONE',  ( 1.387778780781445676E-14, 40.21320343559642652, 5.999999999999996447 ) ) ;
#6581 = DIRECTION ( 'NONE',  ( -0.000000000000000000, -0.000000000000000000, -1.000000000000000000 ) ) ;
#6582 = CARTESIAN_POINT ( 'NONE',  ( -53.25365409304696129, -222.9757987891379685, 73.25790619872482523 ) ) ;
#6583 = CARTESIAN_POINT ( 'NONE',  ( -16.49999999999999289, -120.9522879036832848, 45.92078884797942351 ) ) ;
#6584 = CARTESIAN_POINT ( 'NONE',  ( -63.64218808964506024, -218.0630119241219802, 88.11533740162713002 ) ) ;
#6585 = EDGE_LOOP ( 'NONE', ( #5653, #765, #1722, #2670 ) ) ;
#6586 = EDGE_CURVE ( 'NONE', #5613, #4630, #2396, .T. ) ;
#6587 = ORIENTED_EDGE ( 'NONE', *, *, #4194, .F. ) ;
#6588 = B_SPLINE_CURVE_WITH_KNOTS ( 'NONE', 3,
 ( #7333, #6752, #2025, #257, #149, #6065, #862, #3801, #1365, #3727, #3764, #1476, #1984, #792, #3839, #2598, #3219, #6170, #2487, #4883, #4265, #902, #4382, #4956, #6104, #5568, #2063, #293, #4844, #3260, #6679, #7256, #7180, #1913, #6608, #224, #6720, #4999, #1330, #6031, #827, #753, #3180, #3106, #5455, #185, #1445, #7292, #2530, #3144, #2639, #6136, #5494, #2562, #5528, #7220, #4338, #1948, #4300, #6643, #1057, #5106, #7517, #2178, #2710, #4605, #7480, #2747, #4531, #478, #446, #5062, #6868, #4031, #6906, #7400, #5720, #5028, #3876, #1552, #1626, #4567, #7366, #6212, #364, #1588, #5678, #944, #2218, #3296, #1512, #4448, #401, #3988 ),
 .UNSPECIFIED., .F., .F.,
 ( 4, 2, 2, 2, 1, 1, 2, 2, 2, 2, 2, 1, 1, 1, 2, 2, 2, 2, 2, 1, 1, 1, 1, 1, 2, 2, 2, 2, 2, 2, 2, 2, 2, 1, 1, 1, 1, 1, 2, 2, 2, 2, 2, 1, 1, 1, 2, 2, 2, 2, 2, 1, 1, 2, 2, 2, 4 ),
 ( 0.000000000000000000, 0.06249999999992246480, 0.09374999999988342658, 0.1093749999998637201, 0.1171874999998538669, 0.1210937499998489403, 0.1230468749998462619, 0.1249999999998435696, 0.1874999999997534750, 0.2187499999997080669, 0.2343749999996855016, 0.2421874999996742328, 0.2460937499996684041, 0.2480468749996652678, 0.2490234374996635469, 0.2499999999996617983, 0.3124999999995126121, 0.3437499999994378941, 0.3593749999994005351, 0.3671874999993818278, 0.3710937499993730015, 0.3730468749993685607, 0.3740234374993658406, 0.3745117187493651745, 0.3747558593743645639, 0.3749999999993639532, 0.4374999999993808841, 0.4687499999993893218, 0.4843749999993939848, 0.4999999999993987032, 0.5624999999994173550, 0.5937499999994271249, 0.6093749999994321209, 0.6171874999994338973, 0.6210937499994346744, 0.6230468749994342303, 0.6240234374994351185, 0.6245117187494356736, 0.6247558593744355626, 0.6249999999994354516, 0.6874999999995098365, 0.7187499999995470290, 0.7343749999995660138, 0.7421874999995753397, 0.7460937499995802247, 0.7480468749995824451, 0.7490234374995835553, 0.7499999999995846656, 0.8124999999996914690, 0.8437499999997449818, 0.8593749999997714051, 0.8671874999997841726, 0.8710937499997907230, 0.8730468749997941647, 0.8749999999997974953, 0.9374999999998987477, 1.000000000000000000 ),
 .UNSPECIFIED. ) ;
#6589 = PLANE ( 'NONE',  #5213 ) ;
#6590 = CARTESIAN_POINT ( 'NONE',  ( 17.75121803101545481, -222.9757987891384801, 73.25790619872466891 ) ) ;
#6591 = VERTEX_POINT ( 'NONE', #7100 ) ;
#6592 = CARTESIAN_POINT ( 'NONE',  ( 220.0000000000000000, 56.99999999999999289, 7.000000000000022204 ) ) ;
#6593 = PLANE ( 'NONE',  #5846 ) ;
#6594 = ORIENTED_EDGE ( 'NONE', *, *, #1457, .T. ) ;
#6595 = VECTOR ( 'NONE', #4345, 999.9999999999998863 ) ;
#6596 = EDGE_CURVE ( 'NONE', #959, #3851, #1245, .T. ) ;
#6597 = CARTESIAN_POINT ( 'NONE',  ( -21.50000000000000000, -120.9522879036833558, 45.92078884797940219 ) ) ;
#6598 = FACE_OUTER_BOUND ( 'NONE', #2506, .T. ) ;
#6599 = FACE_OUTER_BOUND ( 'NONE', #6862, .T. ) ;
#6600 = LINE ( 'NONE', #4767, #853 ) ;
#6601 = DIRECTION ( 'NONE',  ( 5.551115123125783935E-17, 1.000000000000000000, -2.214819436045321778E-32 ) ) ;
#6602 = ORIENTED_EDGE ( 'NONE', *, *, #1643, .T. ) ;
#6603 = VECTOR ( 'NONE', #3450, 1000.000000000000000 ) ;
#6604 = SPHERICAL_SURFACE ( 'NONE', #6354, 3.000000000000000000 ) ;
#6605 = CARTESIAN_POINT ( 'NONE',  ( 0.000000000000000000, 0.000000000000000000, -39.99999999999997868 ) ) ;
#6606 = CYLINDRICAL_SURFACE ( 'NONE', #6455, 9.999999999999998224 ) ;
#6607 = EDGE_CURVE ( 'NONE', #3543, #7465, #3279, .T. ) ;
#6608 = CARTESIAN_POINT ( 'NONE',  ( -63.53936842674539065, -223.0630354780872437, 80.15265254803479422 ) ) ;
#6609 = ADVANCED_FACE ( 'NONE', ( #4099 ), #1321, .T. ) ;
#6610 = PLANE ( 'NONE',  #6051 ) ;
#6611 = VERTEX_POINT ( 'NONE', #4289 ) ;
#6612 = ORIENTED_EDGE ( 'NONE', *, *, #6093, .F. ) ;
#6613 = CARTESIAN_POINT ( 'NONE',  ( 188.0000000000000000, -14.00000000000000711, 0.000000000000000000 ) ) ;
#6614 = CARTESIAN_POINT ( 'NONE',  ( 43.50000000000001421, -39.99999999999999289, 0.000000000000000000 ) ) ;
#6615 = CARTESIAN_POINT ( 'NONE',  ( -70.10306686690893230, -220.2280969603149572, 89.90726370123083200 ) ) ;
#6616 = DIRECTION ( 'NONE',  ( 0.000000000000000000, -8.673617379884050263E-16, -1.000000000000000000 ) ) ;
#6617 = CARTESIAN_POINT ( 'NONE',  ( -63.38652985050246969, -218.0628171002711611, 88.70467567798203845 ) ) ;
#6618 = ORIENTED_EDGE ( 'NONE', *, *, #5274, .F. ) ;
#6619 = ORIENTED_EDGE ( 'NONE', *, *, #2199, .T. ) ;
#6620 = EDGE_CURVE ( 'NONE', #4037, #6725, #2518, .T. ) ;
#6621 = FACE_OUTER_BOUND ( 'NONE', #2733, .T. ) ;
#6622 = DIRECTION ( 'NONE',  ( -0.7071067811865513475, 0.000000000000000000, -0.7071067811865435759 ) ) ;
#6623 = ORIENTED_EDGE ( 'NONE', *, *, #4102, .F. ) ;
#6624 = EDGE_CURVE ( 'NONE', #4643, #6889, #2623, .T. ) ;
#6625 = CARTESIAN_POINT ( 'NONE',  ( 36.00000000000000000, 7.347880794884120722E-16, -5.999999999999986677 ) ) ;
#6626 = CYLINDRICAL_SURFACE ( 'NONE', #1656, 10.00000000000000711 ) ;
#6627 = ORIENTED_EDGE ( 'NONE', *, *, #581, .T. ) ;
#6628 = CARTESIAN_POINT ( 'NONE',  ( 192.1021416551216419, -3.000000000000000000, 18.00000000000001421 ) ) ;
#6629 = DIRECTION ( 'NONE',  ( 0.000000000000000000, 1.000000000000000000, 0.000000000000000000 ) ) ;
#6630 = SHAPE_REPRESENTATION_RELATIONSHIP ( 'NONE' , 'NONE' ,  #97, #596 ) ;
#6631 = ADVANCED_FACE ( 'NONE', ( #3755 ), #3643, .F. ) ;
#6632 = DIRECTION ( 'NONE',  ( 5.605193857299270773E-45, 0.000000000000000000, 1.000000000000000000 ) ) ;
#6633 = MECHANICAL_DESIGN_GEOMETRIC_PRESENTATION_REPRESENTATION (  '', ( #3568 ), #2084 ) ;
#6634 = CARTESIAN_POINT ( 'NONE',  ( 2.000000000000001776, 0.000000000000000000, 0.000000000000000000 ) ) ;
#6635 = PRODUCT_DEFINITION ( 'UNKNOWN', '', #800, #6491 ) ;
#6636 = VERTEX_POINT ( 'NONE', #2474 ) ;
#6637 = ORIENTED_EDGE ( 'NONE', *, *, #1954, .F. ) ;
#6638 = VECTOR ( 'NONE', #2906, 1000.000000000000000 ) ;
#6639 = AXIS2_PLACEMENT_3D ( 'NONE', #259, #6681, #1406 ) ;
#6640 = FACE_OUTER_BOUND ( 'NONE', #7379, .T. ) ;
#6641 = FACE_OUTER_BOUND ( 'NONE', #2079, .T. ) ;
#6642 = CARTESIAN_POINT ( 'NONE',  ( 24.99999999999999289, 86.00000000000001421, -1.214306433183764966E-14 ) ) ;
#6643 = CARTESIAN_POINT ( 'NONE',  ( -63.73643367056612874, -223.0630224519699709, 88.93956664432811010 ) ) ;
#6644 = DIRECTION ( 'NONE',  ( 1.000000000000000000, -0.000000000000000000, -0.000000000000000000 ) ) ;
#6645 = VECTOR ( 'NONE', #3409, 1000.000000000000000 ) ;
#6646 = ORIENTED_EDGE ( 'NONE', *, *, #7076, .F. ) ;
#6647 = EDGE_LOOP ( 'NONE', ( #7313, #2273, #7187, #227 ) ) ;
#6648 = AXIS2_PLACEMENT_3D ( 'NONE', #6088, #3277, #811 ) ;
#6649 = DIRECTION ( 'NONE',  ( 5.868966822792466307E-17, 0.9848077530122080203, -0.1736481776669304977 ) ) ;
#6650 = CARTESIAN_POINT ( 'NONE',  ( -26.50000000000003197, 0.000000000000000000, 15.99999999999998579 ) ) ;
#6651 = DIRECTION ( 'NONE',  ( 0.000000000000000000, 0.000000000000000000, -1.000000000000000000 ) ) ;
#6652 = CARTESIAN_POINT ( 'NONE',  ( -61.29878583597043473, -218.0630238806674868, 91.75193312006507540 ) ) ;
#6653 = ORIENTED_EDGE ( 'NONE', *, *, #1553, .T. ) ;
#6654 = EDGE_CURVE ( 'NONE', #7538, #7239, #6331, .T. ) ;
#6655 = EDGE_LOOP ( 'NONE', ( #7343, #1506, #3134, #3059, #2946, #371, #5875, #5634, #3117, #416, #1109, #4791, #3928, #3592 ) ) ;
#6656 = AXIS2_PLACEMENT_3D ( 'NONE', #6605, #790, #222 ) ;
#6657 = CARTESIAN_POINT ( 'NONE',  ( -24.15685424949240456, -108.3431457505074036, 36.34314575050753859 ) ) ;
#6658 = CARTESIAN_POINT ( 'NONE',  ( 10.21539232130207964, -222.1285142276787496, 73.03087698472252498 ) ) ;
#6659 = ORIENTED_EDGE ( 'NONE', *, *, #6113, .T. ) ;
#6660 = LINE ( 'NONE', #4431, #3952 ) ;
#6661 = DIRECTION ( 'NONE',  ( -0.000000000000000000, -1.000000000000000000, -0.000000000000000000 ) ) ;
#6662 = VECTOR ( 'NONE', #6763, 1000.000000000000000 ) ;
#6663 = ORIENTED_EDGE ( 'NONE', *, *, #54, .T. ) ;
#6664 = ADVANCED_FACE ( 'NONE', ( #6598 ), #3126, .T. ) ;
#6665 = DIRECTION ( 'NONE',  ( 0.000000000000000000, 1.301042606982607490E-15, -1.000000000000000000 ) ) ;
#6666 = DIRECTION ( 'NONE',  ( 0.000000000000000000, -1.445602896647337931E-16, -1.000000000000000000 ) ) ;
#6667 = ORIENTED_EDGE ( 'NONE', *, *, #6948, .F. ) ;
#6668 =( BOUNDED_CURVE ( )  B_SPLINE_CURVE ( 3, ( #4373, #7323, #1287, #6017 ),
 .UNSPECIFIED., .F., .T. ) 
 B_SPLINE_CURVE_WITH_KNOTS ( ( 4, 4 ),
 ( 3.839724354387529903, 4.329963465791605515 ),
 .UNSPECIFIED. ) 
 CURVE ( )  GEOMETRIC_REPRESENTATION_ITEM ( )  RATIONAL_B_SPLINE_CURVE ( ( 1.000000000000000000, 0.9800722126984331428, 0.9800722126984331428, 1.000000000000000000 ) ) 
 REPRESENTATION_ITEM ( '' )  );
#6669 = DIRECTION ( 'NONE',  ( 0.000000000000000000, 0.000000000000000000, 1.000000000000000000 ) ) ;
#6670 = FACE_OUTER_BOUND ( 'NONE', #4505, .T. ) ;
#6671 = FACE_OUTER_BOUND ( 'NONE', #5602, .T. ) ;
#6672 = ORIENTED_EDGE ( 'NONE', *, *, #3422, .T. ) ;
#6673 = ADVANCED_FACE ( 'NONE', ( #7209 ), #139, .T. ) ;
#6674 = VECTOR ( 'NONE', #6785, 1000.000000000000000 ) ;
#6675 = CARTESIAN_POINT ( 'NONE',  ( -10.49999999999996980, 0.000000000000000000, -15.99999999999995914 ) ) ;
#6676 = CARTESIAN_POINT ( 'NONE',  ( 0.000000000000000000, -56.99999999999999289, 0.000000000000000000 ) ) ;
#6677 = CARTESIAN_POINT ( 'NONE',  ( 25.00000000000000711, 77.32233047033632545, 4.535533905932713772 ) ) ;
#6678 = CARTESIAN_POINT ( 'NONE',  ( 217.0000000000000000, -15.08392021690038121, 12.00000000000000711 ) ) ;
#6679 = CARTESIAN_POINT ( 'NONE',  ( -63.18650605524960184, -223.0633041053692409, 79.40656603074529585 ) ) ;
#6680 = ORIENTED_EDGE ( 'NONE', *, *, #3745, .T. ) ;
#6681 = DIRECTION ( 'NONE',  ( 1.000000000000000000, 1.853902270198408060E-44, -1.681558157189779738E-44 ) ) ;
#6682 = CIRCLE ( 'NONE', #777, 6.000000000000000000 ) ;
#6683 = AXIS2_PLACEMENT_3D ( 'NONE', #115, #3538, #3035 ) ;
#6684 = ORIENTED_EDGE ( 'NONE', *, *, #713, .F. ) ;
#6685 = EDGE_CURVE ( 'NONE', #5002, #3211, #787, .T. ) ;
#6686 = ORIENTED_EDGE ( 'NONE', *, *, #3553, .T. ) ;
#6687 = CYLINDRICAL_SURFACE ( 'NONE', #1305, 7.000000000000017764 ) ;
#6688 = VECTOR ( 'NONE', #7152, 1000.000000000000000 ) ;
#6689 = FACE_OUTER_BOUND ( 'NONE', #78, .T. ) ;
#6690 = VECTOR ( 'NONE', #6119, 1000.000000000000227 ) ;
#6691 = CARTESIAN_POINT ( 'NONE',  ( -21.50000000000000000, 16.00000000000003553, 42.31370849898488729 ) ) ;
#6692 = CARTESIAN_POINT ( 'NONE',  ( -26.50000000000002487, 16.00000000000007105, 30.68629150101529035 ) ) ;
#6693 = ORIENTED_EDGE ( 'NONE', *, *, #6405, .F. ) ;
#6694 = CIRCLE ( 'NONE', #6329, 3.000000000000000000 ) ;
#6695 = CIRCLE ( 'NONE', #6818, 2.999999999999999112 ) ;
#6696 = VERTEX_POINT ( 'NONE', #1353 ) ;
#6697 = CARTESIAN_POINT ( 'NONE',  ( -14.84314575050762564, -218.0630240738404666, 71.94153218116483117 ) ) ;
#6698 = CARTESIAN_POINT ( 'NONE',  ( 10.51728042240002914, -228.8136496942592260, 74.82215363428539945 ) ) ;
#6699 = ORIENTED_EDGE ( 'NONE', *, *, #2199, .F. ) ;
#6700 = EDGE_CURVE ( 'NONE', #4517, #5471, #5485, .T. ) ;
#6701 = DIRECTION ( 'NONE',  ( 5.605193857299270773E-45, 0.000000000000000000, 1.000000000000000000 ) ) ;
#6702 = FACE_OUTER_BOUND ( 'NONE', #1301, .T. ) ;
#6703 =( BOUNDED_CURVE ( )  B_SPLINE_CURVE ( 3, ( #6281, #4596, #7014, #2323 ),
 .UNSPECIFIED., .F., .T. ) 
 B_SPLINE_CURVE_WITH_KNOTS ( ( 4, 4 ),
 ( -1.776356839400250465E-15, 1.570796326794894782 ),
 .UNSPECIFIED. ) 
 CURVE ( )  GEOMETRIC_REPRESENTATION_ITEM ( )  RATIONAL_B_SPLINE_CURVE ( ( 1.000000000000000000, 0.8047378541243649375, 0.8047378541243649375, 1.000000000000000000 ) ) 
 REPRESENTATION_ITEM ( '' )  );
#6704 = ORIENTED_EDGE ( 'NONE', *, *, #7463, .F. ) ;
#6705 = DIRECTION ( 'NONE',  ( -1.000000000000000000, 0.000000000000000000, -7.663350976776343357E-46 ) ) ;
#6706 = CARTESIAN_POINT ( 'NONE',  ( -64.50000000000000000, -49.37258300203047412, 0.000000000000000000 ) ) ;
#6707 = CYLINDRICAL_SURFACE ( 'NONE', #2141, 8.500000000000007105 ) ;
#6708 = EDGE_LOOP ( 'NONE', ( #4712, #888, #1558, #3300 ) ) ;
#6709 = CYLINDRICAL_SURFACE ( 'NONE', #2845, 25.00000000000000000 ) ;
#6710 = DIRECTION ( 'NONE',  ( 1.000000000000000000, 0.000000000000000000, 0.000000000000000000 ) ) ;
#6711 = CARTESIAN_POINT ( 'NONE',  ( -27.07790214619733860, -113.7796841263389069, 41.77968412633906325 ) ) ;
#6712 = PRODUCT_DEFINITION_SHAPE ( 'NONE', 'NONE',  #4155 ) ;
#6713 = EDGE_LOOP ( 'NONE', ( #5937, #4572 ) ) ;
#6714 = VERTEX_POINT ( 'NONE', #5555 ) ;
#6715 = SHAPE_REPRESENTATION ( 'connecting rod', ( #1914 ), #6340 ) ;
#6716 = AXIS2_PLACEMENT_3D ( 'NONE', #221, #7253, #2022 ) ;
#6717 = CARTESIAN_POINT ( 'NONE',  ( -30.49999999999998579, -218.0630240738404950, 95.20959099461346398 ) ) ;
#6718 = PRESENTATION_STYLE_ASSIGNMENT (( #5526 ) ) ;
#6719 = CARTESIAN_POINT ( 'NONE',  ( 192.1021416551216419, 3.000000000000000000, 18.00000000000001421 ) ) ;
#6720 = CARTESIAN_POINT ( 'NONE',  ( -63.59161903724382370, -223.0630248190201144, 80.27589206438142355 ) ) ;
#6721 = DIRECTION ( 'NONE',  ( -1.000000000000000000, 0.000000000000000000, -0.000000000000000000 ) ) ;
#6722 = CARTESIAN_POINT ( 'NONE',  ( 217.0000000000000000, -56.99999999999999289, 7.000000000000000888 ) ) ;
#6723 = EDGE_CURVE ( 'NONE', #1796, #2680, #3256, .T. ) ;
#6724 = VECTOR ( 'NONE', #4162, 1000.000000000000000 ) ;
#6725 = VERTEX_POINT ( 'NONE', #7170 ) ;
#6726 = VERTEX_POINT ( 'NONE', #5519 ) ;
#6727 = CARTESIAN_POINT ( 'NONE',  ( -53.17910001414514198, -221.3248423084432943, 72.81553374298380277 ) ) ;
#6728 = CIRCLE ( 'NONE', #101, 15.99999999999999645 ) ;
#6729 = PLANE ( 'NONE',  #545 ) ;
#6730 = DIRECTION ( 'NONE',  ( 4.622231866529368100E-33, -2.600005424922769496E-32, 1.000000000000000000 ) ) ;
#6731 = EDGE_CURVE ( 'NONE', #1595, #6262, #4325, .T. ) ;
#6732 = ORIENTED_EDGE ( 'NONE', *, *, #6624, .T. ) ;
#6733 = ORIENTED_EDGE ( 'NONE', *, *, #5469, .F. ) ;
#6734 = LINE ( 'NONE', #5043, #6565 ) ;
#6735 = ORIENTED_EDGE ( 'NONE', *, *, #893, .F. ) ;
#6736 = FACE_OUTER_BOUND ( 'NONE', #7196, .T. ) ;
#6737 = FACE_OUTER_BOUND ( 'NONE', #6082, .T. ) ;
#6738 = ORIENTED_EDGE ( 'NONE', *, *, #2314, .T. ) ;
#6739 = EDGE_CURVE ( 'NONE', #5563, #2614, #3992, .T. ) ;
#6740 = DIRECTION ( 'NONE',  ( -1.000000000000000000, -0.000000000000000000, -0.000000000000000000 ) ) ;
#6741 = CARTESIAN_POINT ( 'NONE',  ( 47.78524365475804103, 26.96414633745969525, 12.74533806390693691 ) ) ;
#6742 = DIRECTION ( 'NONE',  ( 0.000000000000000000, 0.000000000000000000, 1.000000000000000000 ) ) ;
#6743 = EDGE_LOOP ( 'NONE', ( #3596, #382, #6153, #521 ) ) ;
#6744 = CARTESIAN_POINT ( 'NONE',  ( 0.000000000000000000, -2.312964634635744633E-15, 7.000000000000002665 ) ) ;
#6745 = CARTESIAN_POINT ( 'NONE',  ( 2.354181420065691883E-43, 1.714505518806294244E-15, -13.99999999999999822 ) ) ;
#6746 = LINE ( 'NONE', #287, #135 ) ;
#6747 = EDGE_LOOP ( 'NONE', ( #305, #6464, #3827, #2223 ) ) ;
#6748 = EDGE_CURVE ( 'NONE', #3993, #584, #6191, .T. ) ;
#6749 = DIRECTION ( 'NONE',  ( 1.000000000000000000, 0.000000000000000000, 0.000000000000000000 ) ) ;
#6750 = CARTESIAN_POINT ( 'NONE',  ( -18.00000000000000000, 2.204364238465234639E-15, -9.999999999999994671 ) ) ;
#6751 = DIRECTION ( 'NONE',  ( 0.000000000000000000, 0.000000000000000000, -1.000000000000000000 ) ) ;
#6752 = CARTESIAN_POINT ( 'NONE',  ( -53.96146975291424752, -223.0630240738406940, 73.28127814332049184 ) ) ;
#6753 = ORIENTED_EDGE ( 'NONE', *, *, #207, .T. ) ;
#6754 = CARTESIAN_POINT ( 'NONE',  ( 3.000000000000002665, -56.99999999999999289, 7.000000000000000000 ) ) ;
#6755 = VECTOR ( 'NONE', #5679, 1000.000000000000000 ) ;
#6756 = COLOUR_RGB ( '',0.7921568627450980005, 0.8196078431372548767, 0.9333333333333333481 ) ;
#6757 = ORIENTED_EDGE ( 'NONE', *, *, #7481, .T. ) ;
#6758 = EDGE_CURVE ( 'NONE', #2192, #2574, #2011, .T. ) ;
#6759 = ORIENTED_EDGE ( 'NONE', *, *, #7175, .T. ) ;
#6760 = LINE ( 'NONE', #6840, #7206 ) ;
#6761 = CARTESIAN_POINT ( 'NONE',  ( -21.64859110346408144, -111.8253808406378766, 39.82538084063804007 ) ) ;
#6762 = AXIS2_PLACEMENT_3D ( 'NONE', #5206, #7509, #5865 ) ;
#6763 = DIRECTION ( 'NONE',  ( 5.605193857299270773E-45, 0.000000000000000000, 1.000000000000000000 ) ) ;
#6764 = VERTEX_POINT ( 'NONE', #7281 ) ;
#6765 = AXIS2_PLACEMENT_3D ( 'NONE', #6556, #1857, #7203 ) ;
#6766 = ORIENTED_EDGE ( 'NONE', *, *, #7097, .T. ) ;
#6767 = ADVANCED_FACE ( 'NONE', ( #4370 ), #6707, .F. ) ;
#6768 = EDGE_CURVE ( 'NONE', #1052, #1919, #1464, .T. ) ;
#6769 = CARTESIAN_POINT ( 'NONE',  ( 4.000000000000003553, 0.000000000000000000, 1.387778780781445676E-14 ) ) ;
#6770 = ORIENTED_EDGE ( 'NONE', *, *, #4949, .F. ) ;
#6771 = PRODUCT_RELATED_PRODUCT_CATEGORY ( 'part', '', ( #2160 ) ) ;
#6772 = CARTESIAN_POINT ( 'NONE',  ( 217.0000000000000000, 15.08392021690037943, 12.00000000000000711 ) ) ;
#6773 = CARTESIAN_POINT ( 'NONE',  ( 35.00000000000000000, -39.99999999999999289, 10.00000000000000355 ) ) ;
#6774 = ORIENTED_EDGE ( 'NONE', *, *, #1396, .F. ) ;
#6775 = CIRCLE ( 'NONE', #3835, 8.500000000000007105 ) ;
#6776 = ADVANCED_FACE ( 'NONE', ( #3902 ), #4612, .T. ) ;
#6777 = CARTESIAN_POINT ( 'NONE',  ( 209.9999999999999716, 6.000000000000000000, 28.99999999999998579 ) ) ;
#6778 = DIRECTION ( 'NONE',  ( 0.000000000000000000, 0.000000000000000000, 1.000000000000000000 ) ) ;
#6779 = DIRECTION ( 'NONE',  ( 1.000000000000000000, 2.465190328815661892E-32, -9.244463733058732095E-33 ) ) ;
#6780 = ORIENTED_EDGE ( 'NONE', *, *, #3100, .F. ) ;
#6781 = CARTESIAN_POINT ( 'NONE',  ( -71.04530230988100925, -6.071532165918824830E-14, 35.00000000000001421 ) ) ;
#6782 = CIRCLE ( 'NONE', #6903, 3.000000000000001332 ) ;
#6783 = CARTESIAN_POINT ( 'NONE',  ( 47.00000000000000000, -24.98477067547739239, 35.87248741756260983 ) ) ;
#6784 = DIRECTION ( 'NONE',  ( -0.000000000000000000, -0.000000000000000000, 1.000000000000000000 ) ) ;
#6785 = DIRECTION ( 'NONE',  ( -1.000000000000000000, -2.624548829666596736E-30, 9.231085635203017994E-31 ) ) ;
#6786 = ORIENTED_EDGE ( 'NONE', *, *, #7135, .T. ) ;
#6787 = CARTESIAN_POINT ( 'NONE',  ( 200.0000000000000000, -1.853902270198407045E-42, 13.99999999999999822 ) ) ;
#6788 = B_SPLINE_CURVE_WITH_KNOTS ( 'NONE', 3,
 ( #3546, #2423, #1146, #7117, #4815, #4235, #5389, #1303 ),
 .UNSPECIFIED., .F., .F.,
 ( 4, 2, 2, 4 ),
 ( 0.000000000000000000, 0.4819498650539918438, 0.9733208903963990188, 1.000000000000000000 ),
 .UNSPECIFIED. ) ;
#6789 = CARTESIAN_POINT ( 'NONE',  ( -16.49999999999996447, 7.347880794884121708E-16, -6.000000000000000888 ) ) ;
#6790 = PLANE ( 'NONE',  #7267 ) ;
#6791 = CARTESIAN_POINT ( 'NONE',  ( 186.9025342811887924, 8.510922567869524613, 14.99401584891889172 ) ) ;
#6792 = DIRECTION ( 'NONE',  ( 0.000000000000000000, 0.000000000000000000, 1.000000000000000000 ) ) ;
#6793 = CARTESIAN_POINT ( 'NONE',  ( 50.00000000000000000, 0.000000000000000000, 35.00000000000000000 ) ) ;
#6794 = DIRECTION ( 'NONE',  ( -1.000000000000000000, 0.000000000000000000, -7.663350976776343357E-46 ) ) ;
#6795 = ADVANCED_FACE ( 'NONE', ( #5088 ), #2087, .T. ) ;
#6796 = ORIENTED_EDGE ( 'NONE', *, *, #1937, .T. ) ;
#6797 = ORIENTED_EDGE ( 'NONE', *, *, #7525, .F. ) ;
#6798 = DIRECTION ( 'NONE',  ( 0.000000000000000000, 1.301042606982607490E-15, -1.000000000000000000 ) ) ;
#6799 = CARTESIAN_POINT ( 'NONE',  ( -26.49999999999998224, 15.99999999999998579, 96.09122589815608251 ) ) ;
#6800 = CARTESIAN_POINT ( 'NONE',  ( 30.00000000000000000, 0.000000000000000000, 0.000000000000000000 ) ) ;
#6801 = EDGE_CURVE ( 'NONE', #1413, #1433, #3935, .T. ) ;
#6802 = CIRCLE ( 'NONE', #5459, 3.000000000000002665 ) ;
#6803 = EDGE_LOOP ( 'NONE', ( #2922, #1760, #4195, #1340 ) ) ;
#6804 = EDGE_LOOP ( 'NONE', ( #5477, #1526 ) ) ;
#6805 = VECTOR ( 'NONE', #2813, 1000.000000000000000 ) ;
#6806 = CIRCLE ( 'NONE', #7297, 8.500000000000007105 ) ;
#6807 = AXIS2_PLACEMENT_3D ( 'NONE', #454, #7453, #2874 ) ;
#6808 = CARTESIAN_POINT ( 'NONE',  ( -64.50000000000000000, -218.0630240738404950, 71.94153218116483117 ) ) ;
#6809 = ORIENTED_EDGE ( 'NONE', *, *, #4742, .T. ) ;
#6810 = CARTESIAN_POINT ( 'NONE',  ( -23.84314575050760965, -63.65685424949226956, 36.65685424949239035 ) ) ;
#6811 = DIRECTION ( 'NONE',  ( 4.622231866529368100E-33, -2.600005424922769496E-32, 1.000000000000000000 ) ) ;
#6812 = CIRCLE ( 'NONE', #2751, 2.999999999999999112 ) ;
#6813 = COLOUR_RGB ( '',0.7921568627450980005, 0.8196078431372548767, 0.9333333333333333481 ) ;
#6814 = ADVANCED_FACE ( 'NONE', ( #5748, #3405, #3974 ), #3244, .F. ) ;
#6815 = EDGE_LOOP ( 'NONE', ( #7382, #6929, #6824, #2646 ) ) ;
#6816 = CARTESIAN_POINT ( 'NONE',  ( -15.42929891127140962, -112.5545107178312065, 40.55451071783137706 ) ) ;
#6817 = DIRECTION ( 'NONE',  ( 1.078147950931789757E-16, 0.000000000000000000, 1.000000000000000000 ) ) ;
#6818 = AXIS2_PLACEMENT_3D ( 'NONE', #2062, #292, #6751 ) ;
#6819 = ORIENTED_EDGE ( 'NONE', *, *, #181, .F. ) ;
#6820 = CARTESIAN_POINT ( 'NONE',  ( 205.1295982914644185, 11.00000000000001066, 100.9331852405894665 ) ) ;
#6821 = CARTESIAN_POINT ( 'NONE',  ( -60.75121803101544060, -218.1074892565148389, 95.21743140602129074 ) ) ;
#6822 = CYLINDRICAL_SURFACE ( 'NONE', #3819, 8.000000000000007105 ) ;
#6823 = CARTESIAN_POINT ( 'NONE',  ( 188.0000000000000000, 11.00000000000000533, 7.000000000000014211 ) ) ;
#6824 = ORIENTED_EDGE ( 'NONE', *, *, #3893, .T. ) ;
#6825 = EDGE_CURVE ( 'NONE', #797, #7571, #7422, .T. ) ;
#6826 = ORIENTED_EDGE ( 'NONE', *, *, #6120, .F. ) ;
#6827 = AXIS2_PLACEMENT_3D ( 'NONE', #6894, #352, #7437 ) ;
#6828 = DIRECTION ( 'NONE',  ( -0.000000000000000000, 1.000000000000000000, 1.836970198721029934E-16 ) ) ;
#6829 = DIRECTION ( 'NONE',  ( -1.000000000000000000, 5.551115123125783935E-17, -4.237045877651919561E-33 ) ) ;
#6830 = CARTESIAN_POINT ( 'NONE',  ( 50.00000000000000000, 24.00878702352406435, 13.00000000000000888 ) ) ;
#6831 = LINE ( 'NONE', #2827, #6067 ) ;
#6832 = DIRECTION ( 'NONE',  ( 0.000000000000000000, 0.000000000000000000, -1.000000000000000000 ) ) ;
#6833 = CARTESIAN_POINT ( 'NONE',  ( -21.50000000000000000, -99.90626354475344328, 72.90626354475362803 ) ) ;
#6834 = CARTESIAN_POINT ( 'NONE',  ( -55.98581939899504789, -218.0639615485030731, 72.31444438799266550 ) ) ;
#6835 = ORIENTED_EDGE ( 'NONE', *, *, #4324, .F. ) ;
#6836 = AXIS2_PLACEMENT_3D ( 'NONE', #3536, #6496, #2798 ) ;
#6837 = ORIENTED_EDGE ( 'NONE', *, *, #2571, .T. ) ;
#6838 = EDGE_CURVE ( 'NONE', #6889, #4080, #5930, .T. ) ;
#6839 = CARTESIAN_POINT ( 'NONE',  ( 170.0000000000000000, 0.000000000000000000, 0.000000000000000000 ) ) ;
#6840 = CARTESIAN_POINT ( 'NONE',  ( 209.9999999999999716, 6.000000000000000000, 28.99999999999998934 ) ) ;
#6841 = LINE ( 'NONE', #6991, #6690 ) ;
#6842 = LINE ( 'NONE', #6302, #4580 ) ;
#6843 = CIRCLE ( 'NONE', #4148, 17.99999999999999645 ) ;
#6844 = ORIENTED_EDGE ( 'NONE', *, *, #3041, .T. ) ;
#6845 = ORIENTED_EDGE ( 'NONE', *, *, #1814, .T. ) ;
#6846 = AXIS2_PLACEMENT_3D ( 'NONE', #5901, #4796, #7131 ) ;
#6847 = CARTESIAN_POINT ( 'NONE',  ( -26.50000000000003197, -49.37258300203047412, 0.000000000000000000 ) ) ;
#6848 = ORIENTED_EDGE ( 'NONE', *, *, #7127, .T. ) ;
#6849 = CARTESIAN_POINT ( 'NONE',  ( -32.50000000000002132, -104.2695387347598199, 32.26953873475996204 ) ) ;
#6850 = CARTESIAN_POINT ( 'NONE',  ( 200.0000000000000000, 0.000000000000000000, 0.000000000000000000 ) ) ;
#6851 = ORIENTED_EDGE ( 'NONE', *, *, #5263, .F. ) ;
#6852 = EDGE_CURVE ( 'NONE', #3174, #2858, #4860, .T. ) ;
#6853 = EDGE_CURVE ( 'NONE', #2284, #5657, #5103, .T. ) ;
#6854 = CARTESIAN_POINT ( 'NONE',  ( 49.92191802931394307, 24.80301777383411022, 12.93156150603311083 ) ) ;
#6855 = DIRECTION ( 'NONE',  ( -2.465190328815661892E-32, -1.000000000000000000, -1.193489751472043281E-15 ) ) ;
#6856 = VERTEX_POINT ( 'NONE', #3319 ) ;
#6857 =( LENGTH_UNIT ( ) NAMED_UNIT ( * ) SI_UNIT ( .MILLI., .METRE. ) );
#6858 = CARTESIAN_POINT ( 'NONE',  ( -24.00000000000000000, 3.122849337825749433E-15, -9.999999999999994671 ) ) ;
#6859 = CARTESIAN_POINT ( 'NONE',  ( 21.50000000000000000, -218.0630240738404950, 95.20959099461346398 ) ) ;
#6860 = CARTESIAN_POINT ( 'NONE',  ( -26.50000000000000711, -117.1391065123254407, 44.37576177830231217 ) ) ;
#6861 = EDGE_LOOP ( 'NONE', ( #4953, #6845, #310 ) ) ;
#6862 = EDGE_LOOP ( 'NONE', ( #3738, #1188, #4674, #1615 ) ) ;
#6863 = CARTESIAN_POINT ( 'NONE',  ( 220.0000000000000000, -3.000000000000000000, 0.000000000000000000 ) ) ;
#6864 = EDGE_CURVE ( 'NONE', #1604, #258, #1035, .T. ) ;
#6865 = DIRECTION ( 'NONE',  ( 5.605193857299270773E-45, 0.000000000000000000, 1.000000000000000000 ) ) ;
#6866 = EDGE_CURVE ( 'NONE', #1940, #4160, #420, .T. ) ;
#6867 = CARTESIAN_POINT ( 'NONE',  ( 187.7498399038581454, 3.766229566949281349, 16.46159223694064622 ) ) ;
#6868 = CARTESIAN_POINT ( 'NONE',  ( -61.48006764033648608, -223.0630142795953361, 92.57606059409799570 ) ) ;
#6869 = DIRECTION ( 'NONE',  ( 5.551115123125783935E-17, 1.000000000000000000, 5.166928274020107347E-17 ) ) ;
#6870 = CARTESIAN_POINT ( 'NONE',  ( 4.000000000000003553, 0.000000000000000000, 1.387778780781445676E-14 ) ) ;
#6871 = CARTESIAN_POINT ( 'NONE',  ( -63.71456966626824681, -218.0632277174277931, 79.42893510942502644 ) ) ;
#6872 = B_SPLINE_CURVE_WITH_KNOTS ( 'NONE', 3,
 ( #2913, #4658, #4227, #1257 ),
 .UNSPECIFIED., .F., .F.,
 ( 4, 4 ),
 ( 0.000000000000000000, 1.000000000000000000 ),
 .UNSPECIFIED. ) ;
#6873 = EDGE_LOOP ( 'NONE', ( #5481, #7149, #7442, #3141, #6684 ) ) ;
#6874 = ORIENTED_EDGE ( 'NONE', *, *, #1442, .T. ) ;
#6875 = CARTESIAN_POINT ( 'NONE',  ( -29.50000000000000000, -223.0630240738404950, 96.09122589815579829 ) ) ;
#6876 = LINE ( 'NONE', #6175, #2540 ) ;
#6877 = CARTESIAN_POINT ( 'NONE',  ( -26.50000000000002842, -59.83638031753264386, 32.83638031753274333 ) ) ;
#6878 = CARTESIAN_POINT ( 'NONE',  ( 12.50000000000001066, 12.50000000000001066, 4.999999999999995559 ) ) ;
#6879 = CARTESIAN_POINT ( 'NONE',  ( -10.49999999999996803, 0.000000000000000000, 0.000000000000000000 ) ) ;
#6880 = VECTOR ( 'NONE', #2480, 1000.000000000000000 ) ;
#6881 = ORIENTED_EDGE ( 'NONE', *, *, #636, .F. ) ;
#6882 = ORIENTED_EDGE ( 'NONE', *, *, #7295, .F. ) ;
#6883 = VECTOR ( 'NONE', #6032, 1000.000000000000000 ) ;
#6884 = LINE ( 'NONE', #6355, #1520 ) ;
#6885 = ORIENTED_EDGE ( 'NONE', *, *, #571, .T. ) ;
#6886 = CARTESIAN_POINT ( 'NONE',  ( 217.0000000000000000, -6.000000000000000000, 35.00000000000000000 ) ) ;
#6887 = ADVANCED_FACE ( 'NONE', ( #930 ), #3631, .T. ) ;
#6888 = VECTOR ( 'NONE', #4407, 1000.000000000000000 ) ;
#6889 = VERTEX_POINT ( 'NONE', #5665 ) ;
#6890 = CIRCLE ( 'NONE', #2350, 6.000000000000003553 ) ;
#6891 = FACE_OUTER_BOUND ( 'NONE', #1815, .T. ) ;
#6892 = DIRECTION ( 'NONE',  ( 0.000000000000000000, 0.000000000000000000, -1.000000000000000000 ) ) ;
#6893 = ORIENTED_EDGE ( 'NONE', *, *, #7307, .F. ) ;
#6894 = CARTESIAN_POINT ( 'NONE',  ( 0.000000000000000000, 0.000000000000000000, 0.000000000000000000 ) ) ;
#6895 = DIRECTION ( 'NONE',  ( -1.000000000000000000, 0.000000000000000000, -7.663350976776343357E-46 ) ) ;
#6896 = DIRECTION ( 'NONE',  ( 1.000000000000000000, 1.853902270198408060E-44, 1.681558157189780485E-44 ) ) ;
#6897 = DIRECTION ( 'NONE',  ( -0.000000000000000000, 1.000000000000000000, 0.000000000000000000 ) ) ;
#6898 = CIRCLE ( 'NONE', #7511, 3.000000000000000000 ) ;
#6899 = ADVANCED_FACE ( 'NONE', ( #2662, #389, #4437 ), #1004, .F. ) ;
#6900 = EDGE_LOOP ( 'NONE', ( #3757, #4545, #746, #6972 ) ) ;
#6901 = ORIENTED_EDGE ( 'NONE', *, *, #1961, .T. ) ;
#6902 = DIRECTION ( 'NONE',  ( -1.000000000000000000, 0.000000000000000000, -0.000000000000000000 ) ) ;
#6903 = AXIS2_PLACEMENT_3D ( 'NONE', #5168, #437, #933 ) ;
#6904 = CARTESIAN_POINT ( 'NONE',  ( 4.000000000000000000, 0.000000000000000000, 0.000000000000000000 ) ) ;
#6905 = CARTESIAN_POINT ( 'NONE',  ( 188.9082403859883073, 5.724479639934364705, 18.46800072750736987 ) ) ;
#6906 = CARTESIAN_POINT ( 'NONE',  ( -61.41022502515119896, -223.0630231714714569, 92.65062556679446004 ) ) ;
#6907 = CARTESIAN_POINT ( 'NONE',  ( 13.40989346456145093, -223.0630240738405234, 95.79326762286926567 ) ) ;
#6908 = DIRECTION ( 'NONE',  ( 0.000000000000000000, 0.000000000000000000, -1.000000000000000000 ) ) ;
#6909 = CARTESIAN_POINT ( 'NONE',  ( -61.41499871938025024, -218.0631008031258489, 75.68632222678733967 ) ) ;
#6910 = EDGE_CURVE ( 'NONE', #312, #1071, #2165, .T. ) ;
#6911 = ORIENTED_EDGE ( 'NONE', *, *, #1275, .F. ) ;
#6912 = ORIENTED_EDGE ( 'NONE', *, *, #3963, .F. ) ;
#6913 = DIRECTION ( 'NONE',  ( 0.000000000000000000, 0.000000000000000000, 1.000000000000000000 ) ) ;
#6914 = FACE_BOUND ( 'NONE', #3858, .T. ) ;
#6915 = FACE_OUTER_BOUND ( 'NONE', #6023, .T. ) ;
#6916 = CARTESIAN_POINT ( 'NONE',  ( 50.00000000000000000, 24.90486745229362953, 37.17889356869155648 ) ) ;
#6917 = CARTESIAN_POINT ( 'NONE',  ( 2.775557561562891351E-14, 86.00000000000000000, -1.734723475976807094E-15 ) ) ;
#6918 = ADVANCED_FACE ( 'NONE', ( #1575 ), #4090, .T. ) ;
#6919 = ORIENTED_EDGE ( 'NONE', *, *, #3322, .F. ) ;
#6920 = ORIENTED_EDGE ( 'NONE', *, *, #3814, .T. ) ;
#6921 = DIRECTION ( 'NONE',  ( 1.000000000000000000, 2.465190328815661892E-32, -9.244463733058732095E-33 ) ) ;
#6922 = APPLICATION_CONTEXT ( 'automotive_design' ) ;
#6923 = CIRCLE ( 'NONE', #2986, 12.49999999999999645 ) ;
#6924 = FACE_OUTER_BOUND ( 'NONE', #6815, .T. ) ;
#6925 = CIRCLE ( 'NONE', #4348, 9.999999999999996447 ) ;
#6926 = ORIENTED_EDGE ( 'NONE', *, *, #2983, .F. ) ;
#6927 = CARTESIAN_POINT ( 'NONE',  ( -27.51602904742827604, -67.18204818810112045, 40.18204818810124124 ) ) ;
#6928 = CYLINDRICAL_SURFACE ( 'NONE', #6945, 3.000000000000000888 ) ;
#6929 = ORIENTED_EDGE ( 'NONE', *, *, #5550, .F. ) ;
#6930 = AXIS2_PLACEMENT_3D ( 'NONE', #7232, #3194, #7380 ) ;
#6931 = CONICAL_SURFACE ( 'NONE', #5707, 10.00000000000000355, 0.7853981633974500554 ) ;
#6932 = ORIENTED_EDGE ( 'NONE', *, *, #6739, .F. ) ;
#6933 = EDGE_CURVE ( 'NONE', #7420, #5303, #1120, .T. ) ;
#6934 = CARTESIAN_POINT ( 'NONE',  ( -21.50000000000000000, 0.000000000000000000, 0.000000000000000000 ) ) ;
#6935 = VERTEX_POINT ( 'NONE', #1777 ) ;
#6936 = DIRECTION ( 'NONE',  ( 0.6348884888955902417, 9.247752056988617483E-17, 0.7726037837519784679 ) ) ;
#6937 = AXIS2_PLACEMENT_3D ( 'NONE', #6428, #4584, #3354 ) ;
#6938 = CARTESIAN_POINT ( 'NONE',  ( -69.99135978879996856, -227.6251019015761869, 80.18334626974976231 ) ) ;
#6939 = LINE ( 'NONE', #1703, #6645 ) ;
#6940 = AXIS2_PLACEMENT_3D ( 'NONE', #7526, #2267, #2613 ) ;
#6941 = LINE ( 'NONE', #7440, #658 ) ;
#6942 = VERTEX_POINT ( 'NONE', #5281 ) ;
#6943 = ORIENTED_EDGE ( 'NONE', *, *, #6352, .F. ) ;
#6944 = AXIS2_PLACEMENT_3D ( 'NONE', #1372, #2537, #6039 ) ;
#6945 = AXIS2_PLACEMENT_3D ( 'NONE', #2692, #3818, #4512 ) ;
#6946 = AXIS2_PLACEMENT_3D ( 'NONE', #4603, #6949, #6288 ) ;
#6947 = DIRECTION ( 'NONE',  ( -0.7071067811865482389, 0.000000000000000000, 0.7071067811865469066 ) ) ;
#6948 = EDGE_CURVE ( 'NONE', #3617, #4871, #7058, .T. ) ;
#6949 = DIRECTION ( 'NONE',  ( -1.000000000000000000, -1.725633230170963324E-31, 1.078147950931789387E-16 ) ) ;
#6950 = CARTESIAN_POINT ( 'NONE',  ( -64.50000000000000000, 0.000000000000000000, 0.000000000000000000 ) ) ;
#6951 = CARTESIAN_POINT ( 'NONE',  ( 17.92438667413662046, -223.0630240738404950, 76.38511945211442367 ) ) ;
#6952 = DIRECTION ( 'NONE',  ( -4.237045877651920929E-33, -2.600005424922769496E-32, 1.000000000000000000 ) ) ;
#6953 = CARTESIAN_POINT ( 'NONE',  ( -58.71195746406514360, -218.0634440981631599, 73.48571986131535994 ) ) ;
#6954 = ORIENTED_EDGE ( 'NONE', *, *, #5126, .F. ) ;
#6955 = B_SPLINE_CURVE_WITH_KNOTS ( 'NONE', 3,
 ( #1791, #7136, #4145, #1866, #4184, #4220, #3487, #5835, #6561, #6488, #6526, #1248, #633, #1209, #2299, #3604, #3455, #17, #5327, #5942, #63, #5795, #4650, #557, #6984, #7593, #2905, #3564, #5872, #674, #5904, #5256, #5290, #2980, #4066, #3027, #6411, #1131, #7488, #3957, #1518, #1682, #4538 ),
 .UNSPECIFIED., .F., .F.,
 ( 4, 1, 2, 2, 1, 1, 2, 2, 1, 2, 2, 1, 1, 2, 2, 2, 2, 1, 1, 2, 2, 1, 1, 1, 2, 2, 4 ),
 ( 0.000000000000000000, 0.06250000000000000000, 0.09374999999999988898, 0.1249999999999997780, 0.1875000000000000000, 0.2187499999999997780, 0.2343749999999992784, 0.2499999999999987788, 0.3124999999999968359, 0.3437499999999963363, 0.3749999999999958367, 0.4374999999999958367, 0.4687499999999958367, 0.4843749999999952816, 0.4999999999999947264, 0.5624999999999947820, 0.6249999999999947820, 0.6874999999999947820, 0.7187499999999948930, 0.7343749999999948930, 0.7499999999999948930, 0.8124999999999954481, 0.8437499999999962252, 0.8593749999999964473, 0.8671874999999964473, 0.8749999999999964473, 1.000000000000000000 ),
 .UNSPECIFIED. ) ;
#6956 = ORIENTED_EDGE ( 'NONE', *, *, #6254, .F. ) ;
#6957 = CARTESIAN_POINT ( 'NONE',  ( 21.50000000000000000, -6.938893903907228378E-15, 15.99999999999998579 ) ) ;
#6958 = CARTESIAN_POINT ( 'NONE',  ( 12.50000000000001066, 12.50000000000001066, -1.214306433183764966E-14 ) ) ;
#6959 = CARTESIAN_POINT ( 'NONE',  ( 220.0000000000000000, 56.99999999999999289, 10.00000000000002309 ) ) ;
#6960 = DIRECTION ( 'NONE',  ( 0.000000000000000000, 0.9961946980917452121, 0.08715574274766277330 ) ) ;
#6961 = ADVANCED_FACE ( 'NONE', ( #4019 ), #5146, .T. ) ;
#6962 = CARTESIAN_POINT ( 'NONE',  ( -8.500000000000003553, -218.0630240738404666, 44.76505905230349214 ) ) ;
#6963 = ORIENTED_EDGE ( 'NONE', *, *, #2800, .T. ) ;
#6964 = ORIENTED_EDGE ( 'NONE', *, *, #1153, .F. ) ;
#6965 = DIRECTION ( 'NONE',  ( 1.000000000000000000, 4.437342591868191405E-31, -3.379803290564627108E-16 ) ) ;
#6966 = AXIS2_PLACEMENT_3D ( 'NONE', #358, #3911, #3214 ) ;
#6967 = CARTESIAN_POINT ( 'NONE',  ( -26.50000000000003197, 8.628166150854813118E-31, 6.000000000000001776 ) ) ;
#6968 = EDGE_CURVE ( 'NONE', #5372, #2966, #3751, .T. ) ;
#6969 = ORIENTED_EDGE ( 'NONE', *, *, #143, .T. ) ;
#6970 = CARTESIAN_POINT ( 'NONE',  ( 49.45068872151877315, -24.66606923277885599, 10.00000000000000178 ) ) ;
#6971 = CARTESIAN_POINT ( 'NONE',  ( 3.000000000000002665, 30.03170604878415162, 10.00000000000001243 ) ) ;
#6972 = ORIENTED_EDGE ( 'NONE', *, *, #2802, .F. ) ;
#6973 = AXIS2_PLACEMENT_3D ( 'NONE', #2473, #2977, #707 ) ;
#6974 = VERTEX_POINT ( 'NONE', #4317 ) ;
#6975 = CARTESIAN_POINT ( 'NONE',  ( 10.18232950104899537, -221.3963574071737810, 72.83469615593526214 ) ) ;
#6976 = CARTESIAN_POINT ( 'NONE',  ( 27.16044999292957840, -217.6494054747795417, 89.39435792273810932 ) ) ;
#6977 = VERTEX_POINT ( 'NONE', #5436 ) ;
#6978 = CARTESIAN_POINT ( 'NONE',  ( -13.64230087749234599, -110.6367035073516689, 38.63670350735182524 ) ) ;
#6979 = CARTESIAN_POINT ( 'NONE',  ( -32.50000000000002132, -39.68629150101520509, 16.00000000000001421 ) ) ;
#6980 = ORIENTED_EDGE ( 'NONE', *, *, #3135, .F. ) ;
#6981 = EDGE_LOOP ( 'NONE', ( #7503, #1985, #6994, #6091 ) ) ;
#6982 = FACE_OUTER_BOUND ( 'NONE', #1098, .T. ) ;
#6983 = DIRECTION ( 'NONE',  ( -1.000000000000000000, 1.224646799147353454E-16, 0.000000000000000000 ) ) ;
#6984 = CARTESIAN_POINT ( 'NONE',  ( 21.40668666387986718, -218.0630240738405803, 82.00764644045258933 ) ) ;
#6985 = CARTESIAN_POINT ( 'NONE',  ( 11.97238702448635728, -223.0630240738405234, 96.09122589815578408 ) ) ;
#6986 = DIRECTION ( 'NONE',  ( 0.000000000000000000, -1.000000000000000000, -1.221245327087672392E-15 ) ) ;
#6987 = ADVANCED_FACE ( 'NONE', ( #1963 ), #3705, .F. ) ;
#6988 = ORIENTED_EDGE ( 'NONE', *, *, #865, .T. ) ;
#6989 = DIRECTION ( 'NONE',  ( 0.000000000000000000, 0.000000000000000000, 1.000000000000000000 ) ) ;
#6990 = CARTESIAN_POINT ( 'NONE',  ( -16.49999999999998934, -117.9145199278634522, 44.76505905230362714 ) ) ;
#6991 = CARTESIAN_POINT ( 'NONE',  ( 30.00000000000000000, 9.797174393178829602E-16, -8.000000000000003553 ) ) ;
#6992 = DIRECTION ( 'NONE',  ( 0.000000000000000000, -1.000000000000000000, 0.000000000000000000 ) ) ;
#6993 = EDGE_CURVE ( 'NONE', #5598, #2040, #1344, .T. ) ;
#6994 = ORIENTED_EDGE ( 'NONE', *, *, #4623, .F. ) ;
#6995 = ORIENTED_EDGE ( 'NONE', *, *, #3767, .T. ) ;
#6996 = CARTESIAN_POINT ( 'NONE',  ( 27.99999999999998579, 0.000000000000000000, 0.000000000000000000 ) ) ;
#6997 = CARTESIAN_POINT ( 'NONE',  ( 188.0000000000000000, -10.95994505756729254, 7.000000000000017764 ) ) ;
#6998 = ORIENTED_EDGE ( 'NONE', *, *, #911, .F. ) ;
#6999 = CIRCLE ( 'NONE', #248, 6.000000000000001776 ) ;
#7000 = CARTESIAN_POINT ( 'NONE',  ( 49.99999999999999289, -23.17515487249191963, 12.98629252876240514 ) ) ;
#7001 = CARTESIAN_POINT ( 'NONE',  ( -64.50000000000000000, -120.9522879036833274, 45.92078884797940219 ) ) ;
#7002 = ORIENTED_EDGE ( 'NONE', *, *, #713, .T. ) ;
#7003 = AXIS2_PLACEMENT_3D ( 'NONE', #6793, #945, #3297 ) ;
#7004 = ADVANCED_FACE ( 'NONE', ( #2577 ), #4979, .T. ) ;
#7005 = EDGE_CURVE ( 'NONE', #3994, #5048, #4563, .T. ) ;
#7006 = ORIENTED_EDGE ( 'NONE', *, *, #6852, .F. ) ;
#7007 = VECTOR ( 'NONE', #6794, 1000.000000000000000 ) ;
#7008 =( BOUNDED_CURVE ( )  B_SPLINE_CURVE ( 3, ( #559, #1793, #1134, #4687 ),
 .UNSPECIFIED., .F., .T. ) 
 B_SPLINE_CURVE_WITH_KNOTS ( ( 4, 4 ),
 ( 3.926990816987240951, 4.712388980384689674 ),
 .UNSPECIFIED. ) 
 CURVE ( )  GEOMETRIC_REPRESENTATION_ITEM ( )  RATIONAL_B_SPLINE_CURVE ( ( 1.000000000000000000, 0.9492530216741910110, 0.9492530216741910110, 1.000000000000000000 ) ) 
 REPRESENTATION_ITEM ( '' )  );
#7009 = CARTESIAN_POINT ( 'NONE',  ( 49.99999999999999289, 24.00878702352406435, 13.00000000000000711 ) ) ;
#7010 = CARTESIAN_POINT ( 'NONE',  ( 27.21559789597881007, -215.1711607728661022, 88.90143116695426784 ) ) ;
#7011 = ORIENTED_EDGE ( 'NONE', *, *, #336, .T. ) ;
#7012 = APPLICATION_PROTOCOL_DEFINITION ( 'draft international standard', 'automotive_design', 1998, #7413 ) ;
#7013 = AXIS2_PLACEMENT_3D ( 'NONE', #3605, #6632, #6098 ) ;
#7014 = CARTESIAN_POINT ( 'NONE',  ( -26.49999999999998224, -216.4061698243480976, 94.91744288732648727 ) ) ;
#7015 = CARTESIAN_POINT ( 'NONE',  ( -26.50000000000003197, -49.37258300203047412, 0.000000000000000000 ) ) ;
#7016 = ORIENTED_EDGE ( 'NONE', *, *, #3702, .F. ) ;
#7017 = ADVANCED_FACE ( 'NONE', ( #1637, #1066 ), #6383, .F. ) ;
#7018 = AXIS2_PLACEMENT_3D ( 'NONE', #5479, #703, #7128 ) ;
#7019 = CARTESIAN_POINT ( 'NONE',  ( -29.77084236316893140, -74.27084236316864008, 47.27084236316875376 ) ) ;
#7020 = DIRECTION ( 'NONE',  ( 1.000000000000000000, 2.624548829666596736E-30, -9.231085635203017994E-31 ) ) ;
#7021 = PLANE ( 'NONE',  #1528 ) ;
#7022 = DIRECTION ( 'NONE',  ( 5.551115123125786400E-17, 1.000000000000000000, -3.556183125752453755E-15 ) ) ;
#7023 = CYLINDRICAL_SURFACE ( 'NONE', #6518, 2.999999999999999112 ) ;
#7024 = CARTESIAN_POINT ( 'NONE',  ( -10.49999999999996803, -49.37258300203045280, -2.775557561562891351E-14 ) ) ;
#7025 = UNCERTAINTY_MEASURE_WITH_UNIT (LENGTH_MEASURE( 1.000000000000000082E-05 ), #3799, 'distance_accuracy_value', 'NONE');
#7026 = VERTEX_POINT ( 'NONE', #5766 ) ;
#7027 = APPLICATION_CONTEXT ( 'automotive_design' ) ;
#7028 = ORIENTED_EDGE ( 'NONE', *, *, #2137, .T. ) ;
#7029 = DIRECTION ( 'NONE',  ( 0.000000000000000000, 1.000000000000000000, 0.000000000000000000 ) ) ;
#7030 = DIRECTION ( 'NONE',  ( 5.605193857299270773E-45, 0.000000000000000000, 1.000000000000000000 ) ) ;
#7031 = ADVANCED_FACE ( 'NONE', ( #4618 ), #5227, .T. ) ;
#7032 = DIRECTION ( 'NONE',  ( 1.000000000000000000, -5.551115123125783935E-17, 4.237045877651919561E-33 ) ) ;
#7033 = CARTESIAN_POINT ( 'NONE',  ( 1.387778780781445676E-14, 40.21320343559642652, 10.99999999999999467 ) ) ;
#7034 = VERTEX_POINT ( 'NONE', #4577 ) ;
#7035 = ORIENTED_EDGE ( 'NONE', *, *, #4623, .T. ) ;
#7036 = CARTESIAN_POINT ( 'NONE',  ( -21.50000000000000000, -105.5631177942458265, 67.24940929526127320 ) ) ;
#7037 = ADVANCED_FACE ( 'NONE', ( #6915 ), #7410, .F. ) ;
#7038 = FACE_OUTER_BOUND ( 'NONE', #4012, .T. ) ;
#7039 = EDGE_LOOP ( 'NONE', ( #3056, #1854, #3632, #3050 ) ) ;
#7040 = CARTESIAN_POINT ( 'NONE',  ( -21.49999999999999645, -69.31370849898463860, 42.31370849898474518 ) ) ;
#7041 = DIRECTION ( 'NONE',  ( -1.000000000000000000, 0.000000000000000000, -7.663350976776343357E-46 ) ) ;
#7042 = ORIENTED_EDGE ( 'NONE', *, *, #1598, .F. ) ;
#7043 = EDGE_LOOP ( 'NONE', ( #810, #4393, #5387, #2815 ) ) ;
#7044 = DIRECTION ( 'NONE',  ( 0.000000000000000000, -0.08715574274766212104, 0.9961946980917452121 ) ) ;
#7045 = CARTESIAN_POINT ( 'NONE',  ( 10.25365409304695952, -218.1074892565148104, 95.21743140602106337 ) ) ;
#7046 = ORIENTED_EDGE ( 'NONE', *, *, #37, .T. ) ;
#7047 = ITEM_DEFINED_TRANSFORMATION ( 'NONE', 'NONE', #5111,  #1914 ) ;
#7048 = EDGE_CURVE ( 'NONE', #2599, #441, #2519, .T. ) ;
#7049 = FACE_OUTER_BOUND ( 'NONE', #3087, .T. ) ;
#7050 = DIRECTION ( 'NONE',  ( 4.622231866529368100E-33, -2.600005424922769496E-32, 1.000000000000000000 ) ) ;
#7051 = VECTOR ( 'NONE', #2245, 1000.000000000000000 ) ;
#7052 = AXIS2_PLACEMENT_3D ( 'NONE', #565, #5878, #5952 ) ;
#7053 = ORIENTED_EDGE ( 'NONE', *, *, #3641, .T. ) ;
#7054 = DIRECTION ( 'NONE',  ( -5.551115123125785167E-17, 0.7071067811865469066, 0.7071067811865482389 ) ) ;
#7055 = VECTOR ( 'NONE', #2648, 1000.000000000000000 ) ;
#7056 = VECTOR ( 'NONE', #2528, 1000.000000000000114 ) ;
#7057 = CARTESIAN_POINT ( 'NONE',  ( 0.000000000000000000, 0.000000000000000000, -6.999999999999992006 ) ) ;
#7058 = CIRCLE ( 'NONE', #548, 9.999999999999998224 ) ;
#7059 = LINE ( 'NONE', #4100, #3505 ) ;
#7060 = FACE_OUTER_BOUND ( 'NONE', #2632, .T. ) ;
#7061 = EDGE_CURVE ( 'NONE', #3224, #5692, #3820, .T. ) ;
#7062 = CARTESIAN_POINT ( 'NONE',  ( -16.49999999999996447, -6.938893903907228378E-15, 15.99999999999998579 ) ) ;
#7063 = CARTESIAN_POINT ( 'NONE',  ( 0.000000000000000000, -1.445602896647342072E-15, 7.000000000000012434 ) ) ;
#7064 = AXIS2_PLACEMENT_3D ( 'NONE', #2759, #6301, #4541 ) ;
#7065 = VECTOR ( 'NONE', #3072, 1000.000000000000000 ) ;
#7066 = ORIENTED_EDGE ( 'NONE', *, *, #5828, .F. ) ;
#7067 = DIRECTION ( 'NONE',  ( 3.503246160812043455E-46, 0.7071067811865485719, 0.7071067811865464625 ) ) ;
#7068 = CARTESIAN_POINT ( 'NONE',  ( 0.000000000000000000, 0.000000000000000000, 0.000000000000000000 ) ) ;
#7069 = SPHERICAL_SURFACE ( 'NONE', #85, 3.000000000000000000 ) ;
#7070 = CARTESIAN_POINT ( 'NONE',  ( 203.9378221735088630, 3.000000000000000000, 38.49999999999999289 ) ) ;
#7071 = DIRECTION ( 'NONE',  ( 0.000000000000000000, -1.000000000000000000, 0.000000000000000000 ) ) ;
#7072 = AXIS2_PLACEMENT_3D ( 'NONE', #1813, #87, #1654 ) ;
#7073 =( GEOMETRIC_REPRESENTATION_CONTEXT ( 3 ) GLOBAL_UNCERTAINTY_ASSIGNED_CONTEXT ( ( #6022 ) ) GLOBAL_UNIT_ASSIGNED_CONTEXT ( ( #214, #7212, #4989 ) ) REPRESENTATION_CONTEXT ( 'NONE', 'WORKASPACE' ) );
#7074 = CARTESIAN_POINT ( 'NONE',  ( -10.49999999999996980, 16.00000000000012079, -15.99999999999995914 ) ) ;
#7075 = ORIENTED_EDGE ( 'NONE', *, *, #6500, .T. ) ;
#7076 = EDGE_CURVE ( 'NONE', #6725, #5598, #178, .T. ) ;
#7077 = ORIENTED_EDGE ( 'NONE', *, *, #4763, .T. ) ;
#7078 = PRODUCT_DEFINITION_SHAPE ( 'NONE', 'NONE',  #3350 ) ;
#7079 = CARTESIAN_POINT ( 'NONE',  ( 3.000000000000000000, -56.99999999999999289, 7.000000000000000888 ) ) ;
#7080 = CARTESIAN_POINT ( 'NONE',  ( 24.99999999999999289, 86.00000000000001421, 9.999999999999992895 ) ) ;
#7081 = ORIENTED_EDGE ( 'NONE', *, *, #4286, .T. ) ;
#7082 = CARTESIAN_POINT ( 'NONE',  ( -70.12218822116579986, -219.3688186872617507, 89.73635190582676557 ) ) ;
#7083 = AXIS2_PLACEMENT_3D ( 'NONE', #5462, #2536, #4306 ) ;
#7084 = DIRECTION ( 'NONE',  ( 1.681558157189779489E-44, -0.02411877311568873250, 0.9997091000803153271 ) ) ;
#7085 = CARTESIAN_POINT ( 'NONE',  ( 50.00000000000000000, 0.000000000000000000, 60.00000000000000711 ) ) ;
#7086 = ORIENTED_EDGE ( 'NONE', *, *, #6015, .F. ) ;
#7087 = ORIENTED_EDGE ( 'NONE', *, *, #4995, .T. ) ;
#7088 = VECTOR ( 'NONE', #2096, 999.9999999999998863 ) ;
#7089 = CARTESIAN_POINT ( 'NONE',  ( 2.000000000000001776, 0.000000000000000000, 0.000000000000000000 ) ) ;
#7090 = CARTESIAN_POINT ( 'NONE',  ( 17.75121803101545481, -218.1074892565148389, 95.21743140602129074 ) ) ;
#7091 = VERTEX_POINT ( 'NONE', #3429 ) ;
#7092 = CONTEXT_DEPENDENT_SHAPE_REPRESENTATION ( #874, #44 ) ;
#7093 = DIRECTION ( 'NONE',  ( 0.000000000000000000, 0.000000000000000000, 1.000000000000000000 ) ) ;
#7094 = CARTESIAN_POINT ( 'NONE',  ( -32.50000000000002132, -39.68629150101521930, 16.00000000000001421 ) ) ;
#7095 = PRODUCT_DEFINITION_SHAPE ( 'NONE', 'NONE',  #5981 ) ;
#7096 = ORIENTED_EDGE ( 'NONE', *, *, #5690, .F. ) ;
#7097 = EDGE_CURVE ( 'NONE', #5613, #1936, #6841, .T. ) ;
#7098 = CIRCLE ( 'NONE', #1192, 7.999999999999992895 ) ;
#7099 = CYLINDRICAL_SURFACE ( 'NONE', #2794, 9.999999999999996447 ) ;
#7100 = CARTESIAN_POINT ( 'NONE',  ( -13.64230087749234599, -65.63670350735179682, 38.63670350735190340 ) ) ;
#7101 = CARTESIAN_POINT ( 'NONE',  ( 2.775557561562891351E-14, 40.21320343559642652, 0.9999999999999956701 ) ) ;
#7102 = DIRECTION ( 'NONE',  ( 1.000000000000000000, 0.000000000000000000, 0.000000000000000000 ) ) ;
#7103 = CYLINDRICAL_SURFACE ( 'NONE', #4059, 3.000000000000000000 ) ;
#7104 = UNCERTAINTY_MEASURE_WITH_UNIT (LENGTH_MEASURE( 1.000000000000000082E-05 ), #1246, 'distance_accuracy_value', 'NONE');
#7105 = EDGE_CURVE ( 'NONE', #529, #5743, #1684, .T. ) ;
#7106 = ORIENTED_EDGE ( 'NONE', *, *, #3570, .F. ) ;
#7107 = EDGE_CURVE ( 'NONE', #7449, #5598, #7564, .T. ) ;
#7108 = FACE_OUTER_BOUND ( 'NONE', #5780, .T. ) ;
#7109 = CARTESIAN_POINT ( 'NONE',  ( 186.9059892324150383, -5.031373033403107264, 15.00000000000000888 ) ) ;
#7110 = CARTESIAN_POINT ( 'NONE',  ( -10.49999999999997513, -59.26953873475991230, 32.26953873476001888 ) ) ;
#7111 = CARTESIAN_POINT ( 'NONE',  ( 25.00000000000000711, 28.00000000000002487, 4.999999999999995559 ) ) ;
#7112 = DIRECTION ( 'NONE',  ( 0.000000000000000000, 0.000000000000000000, 1.000000000000000000 ) ) ;
#7113 = ORIENTED_EDGE ( 'NONE', *, *, #1165, .T. ) ;
#7114 = PRODUCT_DEFINITION_SHAPE ( 'NONE', 'NONE',  #7603 ) ;
#7115 = EDGE_LOOP ( 'NONE', ( #335, #4967, #7053, #4704, #5621 ) ) ;
#7116 = PLANE ( 'NONE',  #4143 ) ;
#7117 = CARTESIAN_POINT ( 'NONE',  ( -53.33013951010422460, -219.8343230396700392, 95.52191879319023826 ) ) ;
#7118 = ORIENTED_EDGE ( 'NONE', *, *, #197, .T. ) ;
#7119 = CARTESIAN_POINT ( 'NONE',  ( -53.25562355766779632, -223.0194114314941771, 73.26959217102397304 ) ) ;
#7120 = CARTESIAN_POINT ( 'NONE',  ( -63.57333428775314843, -218.0629783339272194, 88.28346941490387678 ) ) ;
#7121 = ORIENTED_EDGE ( 'NONE', *, *, #2605, .T. ) ;
#7122 = ORIENTED_EDGE ( 'NONE', *, *, #1306, .T. ) ;
#7123 = DIRECTION ( 'NONE',  ( 1.000000000000000000, 0.000000000000000000, 5.605193857299269528E-45 ) ) ;
#7124 = CARTESIAN_POINT ( 'NONE',  ( 10.25562355766779277, -223.0194114314941203, 73.26959217102397304 ) ) ;
#7125 = ORIENTED_EDGE ( 'NONE', *, *, #1542, .T. ) ;
#7126 = SHAPE_DEFINITION_REPRESENTATION ( #7095, #6475 ) ;
#7127 = EDGE_CURVE ( 'NONE', #7386, #5895, #60, .T. ) ;
#7128 = DIRECTION ( 'NONE',  ( 0.000000000000000000, 0.000000000000000000, -1.000000000000000000 ) ) ;
#7129 = DIRECTION ( 'NONE',  ( -1.000000000000000000, 0.000000000000000000, -0.000000000000000000 ) ) ;
#7130 = ORIENTED_EDGE ( 'NONE', *, *, #5840, .T. ) ;
#7131 = DIRECTION ( 'NONE',  ( 0.000000000000000000, 0.000000000000000000, -1.000000000000000000 ) ) ;
#7132 = AXIS2_PLACEMENT_3D ( 'NONE', #4479, #1579, #4441 ) ;
#7133 = CARTESIAN_POINT ( 'NONE',  ( 50.00000000000000000, 24.00878702352406435, 13.00000000000000888 ) ) ;
#7134 = FACE_OUTER_BOUND ( 'NONE', #7308, .T. ) ;
#7135 = EDGE_CURVE ( 'NONE', #5727, #5611, #1717, .T. ) ;
#7136 = CARTESIAN_POINT ( 'NONE',  ( 11.01479902034195746, -218.0630240738405234, 95.20959099461350661 ) ) ;
#7137 = CARTESIAN_POINT ( 'NONE',  ( 176.5000000000000000, 39.99999999999999289, 0.000000000000000000 ) ) ;
#7138 = DIRECTION ( 'NONE',  ( -1.000000000000000000, 1.294224922628222493E-31, -1.078147950931789264E-16 ) ) ;
#7139 = VECTOR ( 'NONE', #6122, 1000.000000000000000 ) ;
#7140 = LINE ( 'NONE', #3685, #1808 ) ;
#7141 = DIRECTION ( 'NONE',  ( 0.000000000000000000, 1.000000000000000000, 1.734723475976805517E-15 ) ) ;
#7142 = DIRECTION ( 'NONE',  ( 0.000000000000000000, 1.301042606982600785E-15, -1.000000000000000000 ) ) ;
#7143 = DIRECTION ( 'NONE',  ( 0.000000000000000000, 0.000000000000000000, 1.000000000000000000 ) ) ;
#7144 = CARTESIAN_POINT ( 'NONE',  ( 188.1399229816385628, 8.449061396769250720, 15.00000000000000888 ) ) ;
#7145=STYLED_ITEM('',(#7631),#1202);
#7146 = CARTESIAN_POINT ( 'NONE',  ( 186.9827202257732779, -7.949242328481256337, 15.13290197900971634 ) ) ;
#7147 = EDGE_CURVE ( 'NONE', #1634, #496, #2836, .T. ) ;
#7148 = ORIENTED_EDGE ( 'NONE', *, *, #7404, .F. ) ;
#7149 = ORIENTED_EDGE ( 'NONE', *, *, #7238, .F. ) ;
#7150 = CARTESIAN_POINT ( 'NONE',  ( -26.50000000000003197, -60.68629150101524772, -11.31370849898474873 ) ) ;
#7151 = AXIS2_PLACEMENT_3D ( 'NONE', #6962, #5733, #2308 ) ;
#7152 = DIRECTION ( 'NONE',  ( 0.5773502691896311712, 0.5773502691896222894, -0.5773502691896238437 ) ) ;
#7153 = CARTESIAN_POINT ( 'NONE',  ( -70.12218822116579986, -221.8025471834170332, 78.75851208262513126 ) ) ;
#7154 = DIRECTION ( 'NONE',  ( 7.623657272262517133E-17, 0.7071067811865465735, -0.7071067811865485719 ) ) ;
#7155 = EDGE_CURVE ( 'NONE', #7026, #5645, #2021, .T. ) ;
#7156 = CARTESIAN_POINT ( 'NONE',  ( -63.51202228486167911, -218.0629290329284515, 88.42502795811738281 ) ) ;
#7157 = EDGE_CURVE ( 'NONE', #5755, #5359, #3880, .T. ) ;
#7158 = EDGE_LOOP ( 'NONE', ( #6205, #6218 ) ) ;
#7159 = ORIENTED_EDGE ( 'NONE', *, *, #1851, .T. ) ;
#7160 = DIRECTION ( 'NONE',  ( 5.605193857299270773E-45, 0.000000000000000000, 1.000000000000000000 ) ) ;
#7161 = CARTESIAN_POINT ( 'NONE',  ( 10.50256896896200409, -228.4878731603044741, 74.73486207509921542 ) ) ;
#7162 = ORIENTED_EDGE ( 'NONE', *, *, #91, .F. ) ;
#7163 = FACE_OUTER_BOUND ( 'NONE', #5712, .T. ) ;
#7164 = FACE_OUTER_BOUND ( 'NONE', #3693, .T. ) ;
#7165 = ORIENTED_EDGE ( 'NONE', *, *, #3720, .F. ) ;
#7166 = AXIS2_PLACEMENT_3D ( 'NONE', #7015, #7549, #4212 ) ;
#7167 = EDGE_CURVE ( 'NONE', #4378, #628, #5688, .T. ) ;
#7168 = EDGE_CURVE ( 'NONE', #5737, #2583, #2188, .T. ) ;
#7169 = CARTESIAN_POINT ( 'NONE',  ( 3.000000000000000000, -21.98659819442010388, 35.76778892745510063 ) ) ;
#7170 = CARTESIAN_POINT ( 'NONE',  ( 1.387778780781445676E-14, 101.5000000000000000, -1.734723475976807094E-15 ) ) ;
#7171 = PLANE ( 'NONE',  #6423 ) ;
#7172 = AXIS2_PLACEMENT_3D ( 'NONE', #7523, #5686, #3920 ) ;
#7173 = PLANE ( 'NONE',  #5161 ) ;
#7174 = ORIENTED_EDGE ( 'NONE', *, *, #6968, .F. ) ;
#7175 = EDGE_CURVE ( 'NONE', #2821, #647, #27, .T. ) ;
#7176 = AXIS2_PLACEMENT_3D ( 'NONE', #484, #2144, #4498 ) ;
#7177 = DIRECTION ( 'NONE',  ( 5.605193857299270773E-45, 0.000000000000000000, 1.000000000000000000 ) ) ;
#7178 = CARTESIAN_POINT ( 'NONE',  ( 0.000000000000000000, 0.000000000000000000, -39.99999999999997868 ) ) ;
#7179 = DIRECTION ( 'NONE',  ( -1.000000000000000000, 5.551115123125783935E-17, -4.237045877651919561E-33 ) ) ;
#7180 = CARTESIAN_POINT ( 'NONE',  ( -63.40503953359656464, -223.0631132561157131, 79.85303703543833365 ) ) ;
#7181 = CARTESIAN_POINT ( 'NONE',  ( 189.9732893686090449, -6.600999473907240400, 16.15635983897348282 ) ) ;
#7182 = VECTOR ( 'NONE', #879, 1000.000000000000000 ) ;
#7183 = AXIS2_PLACEMENT_3D ( 'NONE', #3836, #6168, #2672 ) ;
#7184 = AXIS2_PLACEMENT_3D ( 'NONE', #768, #4864, #6622 ) ;
#7185 = ORIENTED_EDGE ( 'NONE', *, *, #6293, .T. ) ;
#7186 = EDGE_CURVE ( 'NONE', #2809, #4344, #148, .T. ) ;
#7187 = ORIENTED_EDGE ( 'NONE', *, *, #921, .T. ) ;
#7188 = AXIS2_PLACEMENT_3D ( 'NONE', #1892, #812, #4284 ) ;
#7189 = ADVANCED_FACE ( 'NONE', ( #2486 ), #73, .F. ) ;
#7190 = AXIS2_PLACEMENT_3D ( 'NONE', #5677, #2745, #5105 ) ;
#7191 = FACE_BOUND ( 'NONE', #728, .T. ) ;
#7192 = CARTESIAN_POINT ( 'NONE',  ( -53.47314606205194565, -223.0630240738404950, 96.09122589815579829 ) ) ;
#7193 = CARTESIAN_POINT ( 'NONE',  ( -53.10580595754475297, -219.7017882839730873, 72.38063772785491778 ) ) ;
#7194 = CARTESIAN_POINT ( 'NONE',  ( 26.99999999999999289, 0.000000000000000000, -6.999999999999992006 ) ) ;
#7195 = CARTESIAN_POINT ( 'NONE',  ( -63.88876000171747904, -218.0630240738404950, 87.48027644629948441 ) ) ;
#7196 = EDGE_LOOP ( 'NONE', ( #6882, #7162, #5396, #7006 ) ) ;
#7197 = ORIENTED_EDGE ( 'NONE', *, *, #6289, .F. ) ;
#7198 = EDGE_CURVE ( 'NONE', #1310, #3769, #3390, .T. ) ;
#7199 = DIRECTION ( 'NONE',  ( 1.000000000000000000, 0.000000000000000000, 0.000000000000000000 ) ) ;
#7200 = CARTESIAN_POINT ( 'NONE',  ( 17.82928583850155135, -228.1620966263573393, 74.64757051591656989 ) ) ;
#7201 = VERTEX_POINT ( 'NONE', #4226 ) ;
#7202 = PRODUCT_DEFINITION ( 'UNKNOWN', '', #1168, #5260 ) ;
#7203 = DIRECTION ( 'NONE',  ( 0.000000000000000000, 0.000000000000000000, -1.000000000000000000 ) ) ;
#7204 = FACE_BOUND ( 'NONE', #4903, .T. ) ;
#7205 = VERTEX_POINT ( 'NONE', #564 ) ;
#7206 = VECTOR ( 'NONE', #7300, 1000.000000000000000 ) ;
#7207 = DIRECTION ( 'NONE',  ( 0.000000000000000000, 0.000000000000000000, -1.000000000000000000 ) ) ;
#7208 = ADVANCED_BREP_SHAPE_REPRESENTATION ( '', ( #1202, #1914 ), #5724 ) ;
#7209 = FACE_OUTER_BOUND ( 'NONE', #541, .T. ) ;
#7210 = ORIENTED_EDGE ( 'NONE', *, *, #909, .F. ) ;
#7211 = VECTOR ( 'NONE', #3329, 1000.000000000000000 ) ;
#7212 =( NAMED_UNIT ( * ) PLANE_ANGLE_UNIT ( ) SI_UNIT ( $, .RADIAN. ) );
#7213 = CARTESIAN_POINT ( 'NONE',  ( 26.00000000000000000, 0.000000000000000000, 0.000000000000000000 ) ) ;
#7214 = DIRECTION ( 'NONE',  ( 1.853902270198407313E-44, 1.000000000000000000, 0.000000000000000000 ) ) ;
#7215 = ORIENTED_EDGE ( 'NONE', *, *, #2213, .T. ) ;
#7216 = VECTOR ( 'NONE', #6947, 999.9999999999998863 ) ;
#7217 = DIRECTION ( 'NONE',  ( -1.000000000000000000, 0.000000000000000000, 0.000000000000000000 ) ) ;
#7218 = CARTESIAN_POINT ( 'NONE',  ( 1.387778780781445676E-14, 77.32233047033629703, 4.535533905932711995 ) ) ;
#7219 = LINE ( 'NONE', #1092, #5473 ) ;
#7220 = CARTESIAN_POINT ( 'NONE',  ( -63.83803158340868578, -223.0628179935395963, 88.66427253312173207 ) ) ;
#7221 = CARTESIAN_POINT ( 'NONE',  ( -53.25759302228803449, -223.0630240738404950, 73.28127814332044920 ) ) ;
#7222 = EDGE_CURVE ( 'NONE', #5579, #6726, #6332, .T. ) ;
#7223 = ORIENTED_EDGE ( 'NONE', *, *, #6450, .F. ) ;
#7224 = VERTEX_POINT ( 'NONE', #4191 ) ;
#7225 = CARTESIAN_POINT ( 'NONE',  ( -26.50000000000002487, 16.00000000000012079, -15.99999999999995914 ) ) ;
#7226 = CARTESIAN_POINT ( 'NONE',  ( -21.51784377693468642, -113.7796841263389069, 41.77968412633906325 ) ) ;
#7227 = CARTESIAN_POINT ( 'NONE',  ( 220.0000000000000000, -20.99999999999999645, 13.00000000000000888 ) ) ;
#7228 = EDGE_CURVE ( 'NONE', #3811, #2618, #4843, .T. ) ;
#7229 = DIRECTION ( 'NONE',  ( 1.000000000000000000, 0.000000000000000000, 0.000000000000000000 ) ) ;
#7230 = ORIENTED_EDGE ( 'NONE', *, *, #3797, .T. ) ;
#7231 = EDGE_LOOP ( 'NONE', ( #6456, #2455, #996, #4513 ) ) ;
#7232 = CARTESIAN_POINT ( 'NONE',  ( 200.0000000000000000, 0.000000000000000000, 0.000000000000000000 ) ) ;
#7233 = CARTESIAN_POINT ( 'NONE',  ( 2.000000000000001776, -4.163336342344337027E-14, 0.000000000000000000 ) ) ;
#7234 = ORIENTED_EDGE ( 'NONE', *, *, #6546, .F. ) ;
#7235 = CARTESIAN_POINT ( 'NONE',  ( 217.0000000000000000, 15.08392021690037943, 12.00000000000000711 ) ) ;
#7236 = DIRECTION ( 'NONE',  ( 1.000000000000000000, 0.000000000000000000, 0.000000000000000000 ) ) ;
#7237 = EDGE_CURVE ( 'NONE', #5235, #3401, #4074, .T. ) ;
#7238 = EDGE_CURVE ( 'NONE', #510, #7201, #3263, .T. ) ;
#7239 = VERTEX_POINT ( 'NONE', #1179 ) ;
#7240 = CARTESIAN_POINT ( 'NONE',  ( -10.49999999999996803, 0.000000000000000000, 0.000000000000000000 ) ) ;
#7241 = CARTESIAN_POINT ( 'NONE',  ( 50.00000000000000000, 25.78625927331255951, 12.84683604381136668 ) ) ;
#7242 = ORIENTED_EDGE ( 'NONE', *, *, #124, .T. ) ;
#7243 = CARTESIAN_POINT ( 'NONE',  ( 25.00000000000000000, 40.21320343559644783, 10.99999999999999467 ) ) ;
#7244 = LINE ( 'NONE', #5408, #7259 ) ;
#7245 = VECTOR ( 'NONE', #6986, 1000.000000000000000 ) ;
#7246 = DIRECTION ( 'NONE',  ( 2.465190328815661892E-32, 0.7071067811865465735, -0.7071067811865484609 ) ) ;
#7247 = EDGE_CURVE ( 'NONE', #2578, #6174, #1782, .T. ) ;
#7248 = ORIENTED_EDGE ( 'NONE', *, *, #1947, .T. ) ;
#7249 = EDGE_LOOP ( 'NONE', ( #7461, #1837 ) ) ;
#7250 = VECTOR ( 'NONE', #5873, 1000.000000000000000 ) ;
#7251 = AXIS2_PLACEMENT_3D ( 'NONE', #3262, #2676, #5570 ) ;
#7252 = SHAPE_REPRESENTATION ( 'right arm', ( #1914 ), #6207 ) ;
#7253 = DIRECTION ( 'NONE',  ( 0.000000000000000000, 0.000000000000000000, 1.000000000000000000 ) ) ;
#7254 = DIRECTION ( 'NONE',  ( 1.000000000000000000, 0.000000000000000000, 0.000000000000000000 ) ) ;
#7255 = PLANE ( 'NONE',  #4121 ) ;
#7256 = CARTESIAN_POINT ( 'NONE',  ( -63.27605943754021922, -223.0632182441923703, 79.58247367488434065 ) ) ;
#7257 = VERTEX_POINT ( 'NONE', #1296 ) ;
#7258 = CARTESIAN_POINT ( 'NONE',  ( 6.500000000000009770, 12.50000000000001243, -1.214306433183764966E-14 ) ) ;
#7259 = VECTOR ( 'NONE', #745, 1000.000000000000000 ) ;
#7260 = ORIENTED_EDGE ( 'NONE', *, *, #363, .T. ) ;
#7261 = ORIENTED_EDGE ( 'NONE', *, *, #2161, .F. ) ;
#7262 = EDGE_CURVE ( 'NONE', #2069, #2279, #6128, .T. ) ;
#7263 = CIRCLE ( 'NONE', #1479, 5.999999999999999112 ) ;
#7264 = CARTESIAN_POINT ( 'NONE',  ( 200.0000000000000000, 1.714505518806294835E-15, -14.00000000000000533 ) ) ;
#7265 = LINE ( 'NONE', #6614, #1398 ) ;
#7266 = LINE ( 'NONE', #6691, #2851 ) ;
#7267 = AXIS2_PLACEMENT_3D ( 'NONE', #1510, #5675, #2744 ) ;
#7268 = LINE ( 'NONE', #6692, #799 ) ;
#7269 = VERTEX_POINT ( 'NONE', #2949 ) ;
#7270 = ORIENTED_EDGE ( 'NONE', *, *, #1082, .T. ) ;
#7271 = CIRCLE ( 'NONE', #3962, 6.000000000000000000 ) ;
#7272 = DIRECTION ( 'NONE',  ( 1.000000000000000000, 0.000000000000000000, 0.000000000000000000 ) ) ;
#7273 = CARTESIAN_POINT ( 'NONE',  ( 26.99871551551808579, -227.2977332969690281, 80.10323607719463723 ) ) ;
#7274 = VERTEX_POINT ( 'NONE', #1833 ) ;
#7275 = FACE_OUTER_BOUND ( 'NONE', #3778, .T. ) ;
#7276 = CARTESIAN_POINT ( 'NONE',  ( 209.9999999999999716, 6.000000000000000000, 35.00000000000000000 ) ) ;
#7277 = ORIENTED_EDGE ( 'NONE', *, *, #4663, .T. ) ;
#7278 = CARTESIAN_POINT ( 'NONE',  ( 220.0000000000000000, -18.04196010845019060, 12.50000000000000711 ) ) ;
#7279 = ADVANCED_FACE ( 'NONE', ( #643 ), #1256, .T. ) ;
#7280 = CARTESIAN_POINT ( 'NONE',  ( -64.50000000000000000, -223.0630240738404950, 73.28127814332044920 ) ) ;
#7281 = CARTESIAN_POINT ( 'NONE',  ( 170.0000000000000000, -11.00000000000000355, 8.660254037844387298 ) ) ;
#7282 = EDGE_LOOP ( 'NONE', ( #4181, #3965, #1795, #6693 ) ) ;
#7283 =( NAMED_UNIT ( * ) SI_UNIT ( $, .STERADIAN. ) SOLID_ANGLE_UNIT ( ) );
#7284 = DIRECTION ( 'NONE',  ( -5.551115123125783935E-17, -1.000000000000000000, -5.166928274020107963E-17 ) ) ;
#7285 = CARTESIAN_POINT ( 'NONE',  ( 6.938893903907228378E-15, 73.78679656440351664, 10.99999999999999467 ) ) ;
#7286 = CARTESIAN_POINT ( 'NONE',  ( 201.3397459621555470, 6.000000000000000000, 39.99999999999999289 ) ) ;
#7287 = ORIENTED_EDGE ( 'NONE', *, *, #4295, .T. ) ;
#7288 = DIRECTION ( 'NONE',  ( 0.000000000000000000, 0.000000000000000000, 1.000000000000000000 ) ) ;
#7289 = CIRCLE ( 'NONE', #53, 3.000000000000000000 ) ;
#7290 = ADVANCED_FACE ( 'NONE', ( #5951 ), #681, .T. ) ;
#7291 = DIRECTION ( 'NONE',  ( 1.000000000000000000, 2.465190328815661892E-32, -9.244463733058732095E-33 ) ) ;
#7292 = CARTESIAN_POINT ( 'NONE',  ( -64.48438679943396323, -223.0632018673171331, 84.15020320440139301 ) ) ;
#7293 = DIRECTION ( 'NONE',  ( 0.000000000000000000, 0.000000000000000000, 1.000000000000000000 ) ) ;
#7294 = CARTESIAN_POINT ( 'NONE',  ( -12.50000000000001066, -214.0630240738404382, 96.09122589815579829 ) ) ;
#7295 = EDGE_CURVE ( 'NONE', #1796, #3174, #4002, .T. ) ;
#7296 = VECTOR ( 'NONE', #7044, 1000.000000000000000 ) ;
#7297 = AXIS2_PLACEMENT_3D ( 'NONE', #7451, #988, #408 ) ;
#7298 = ORIENTED_EDGE ( 'NONE', *, *, #7361, .F. ) ;
#7299 = ORIENTED_EDGE ( 'NONE', *, *, #5163, .F. ) ;
#7300 = DIRECTION ( 'NONE',  ( -0.000000000000000000, -1.000000000000000000, -0.000000000000000000 ) ) ;
#7301 = AXIS2_PLACEMENT_3D ( 'NONE', #82, #3663, #3621 ) ;
#7302 = DIRECTION ( 'NONE',  ( 0.000000000000000000, 0.000000000000000000, -1.000000000000000000 ) ) ;
#7303 = AXIS2_PLACEMENT_3D ( 'NONE', #4180, #5939, #1129 ) ;
#7304 = VECTOR ( 'NONE', #6779, 1000.000000000000000 ) ;
#7305 = PLANE ( 'NONE',  #1007 ) ;
#7306 = DIRECTION ( 'NONE',  ( 1.000000000000000000, 1.853902270198408060E-44, -1.681558157189779738E-44 ) ) ;
#7307 = EDGE_CURVE ( 'NONE', #2574, #4244, #5266, .T. ) ;
#7308 = EDGE_LOOP ( 'NONE', ( #4056, #1621, #5204, #6627 ) ) ;
#7309 = TOROIDAL_SURFACE ( 'NONE', #3997, 6.000000000000000000, 3.000000000000000000 ) ;
#7310 = CIRCLE ( 'NONE', #2765, 9.999999999999998224 ) ;
#7311 = ORIENTED_EDGE ( 'NONE', *, *, #3447, .F. ) ;
#7312 = CARTESIAN_POINT ( 'NONE',  ( 50.04196010845020481, 18.04196010845019060, 12.50000000000000711 ) ) ;
#7313 = ORIENTED_EDGE ( 'NONE', *, *, #6395, .F. ) ;
#7314 = DIRECTION ( 'NONE',  ( 0.000000000000000000, -1.000000000000000000, -1.836970198721029934E-16 ) ) ;
#7315 = PRODUCT_DEFINITION_FORMATION_WITH_SPECIFIED_SOURCE ( 'ANY', '', #5293, .NOT_KNOWN. ) ;
#7316 = DIRECTION ( 'NONE',  ( 1.000000000000000000, -4.067564042545842122E-31, 3.379803290564626122E-16 ) ) ;
#7317 = ADVANCED_FACE ( 'NONE', ( #4805 ), #4869, .T. ) ;
#7318 = ORIENTED_EDGE ( 'NONE', *, *, #3585, .F. ) ;
#7319 = DIRECTION ( 'NONE',  ( 5.551115123125783935E-17, 1.000000000000000000, -2.214819436045321778E-32 ) ) ;
#7320 = CARTESIAN_POINT ( 'NONE',  ( 186.9059892324150383, 5.031373033403108153, 15.00000000000000888 ) ) ;
#7321 = CARTESIAN_POINT ( 'NONE',  ( 220.0000000000000000, 60.00000000000000000, 10.00000000000002309 ) ) ;
#7322 = ORIENTED_EDGE ( 'NONE', *, *, #3130, .F. ) ;
#7323 = CARTESIAN_POINT ( 'NONE',  ( -28.34608510185598718, -111.4855484589742645, 39.48554845897440657 ) ) ;
#7324 = DIRECTION ( 'NONE',  ( -1.000000000000000000, 0.000000000000000000, -7.663350976776343357E-46 ) ) ;
#7325 = DIRECTION ( 'NONE',  ( -5.605193857299269528E-45, 0.000000000000000000, 1.000000000000000000 ) ) ;
#7326 = VECTOR ( 'NONE', #3343, 1000.000000000000000 ) ;
#7327 = EDGE_CURVE ( 'NONE', #908, #5074, #7598, .T. ) ;
#7328 = ADVANCED_FACE ( 'NONE', ( #4413 ), #6606, .T. ) ;
#7329 = ORIENTED_EDGE ( 'NONE', *, *, #1342, .F. ) ;
#7330 = CIRCLE ( 'NONE', #4024, 6.000000000000001776 ) ;
#7331 = LINE ( 'NONE', #4410, #1311 ) ;
#7332 = CARTESIAN_POINT ( 'NONE',  ( 3.000000000000002665, -28.78532416918554304, 10.00000000000000711 ) ) ;
#7333 = CARTESIAN_POINT ( 'NONE',  ( -53.25759302228803449, -223.0630240738404950, 73.28127814332044920 ) ) ;
#7334 = DIRECTION ( 'NONE',  ( -5.605193857299270773E-45, -0.000000000000000000, -1.000000000000000000 ) ) ;
#7335 = LINE ( 'NONE', #2027, #4 ) ;
#7336 = AXIS2_PLACEMENT_3D ( 'NONE', #5370, #3060, #57 ) ;
#7337 = EDGE_CURVE ( 'NONE', #2926, #2183, #3800, .T. ) ;
#7338 = ADVANCED_FACE ( 'NONE', ( #3179 ), #4381, .F. ) ;
#7339 = VERTEX_POINT ( 'NONE', #255 ) ;
#7340 = ORIENTED_EDGE ( 'NONE', *, *, #4594, .F. ) ;
#7341 = DIRECTION ( 'NONE',  ( 1.000000000000000000, 0.000000000000000000, 0.000000000000000000 ) ) ;
#7342 = DIRECTION ( 'NONE',  ( 0.000000000000000000, 0.000000000000000000, -1.000000000000000000 ) ) ;
#7343 = ORIENTED_EDGE ( 'NONE', *, *, #5374, .T. ) ;
#7344 = ORIENTED_EDGE ( 'NONE', *, *, #1927, .F. ) ;
#7345 = LINE ( 'NONE', #4972, #5838 ) ;
#7346 = EDGE_LOOP ( 'NONE', ( #638, #7512 ) ) ;
#7347 = CARTESIAN_POINT ( 'NONE',  ( 25.00000000000001421, 35.07106781186547551, 2.928932188134525827 ) ) ;
#7348 = DIRECTION ( 'NONE',  ( 1.000000000000000000, 0.000000000000000000, 0.000000000000000000 ) ) ;
#7349 = VERTEX_POINT ( 'NONE', #5567 ) ;
#7350 = LINE ( 'NONE', #7495, #6484 ) ;
#7351 = ADVANCED_FACE ( 'NONE', ( #861 ), #2597, .T. ) ;
#7352 = CARTESIAN_POINT ( 'NONE',  ( -30.49999999999999289, -218.0630240738404950, 71.94153218116483117 ) ) ;
#7353 = CARTESIAN_POINT ( 'NONE',  ( 217.0000000000000000, -9.000000000000001776, 18.00000000000001066 ) ) ;
#7354 = ORIENTED_EDGE ( 'NONE', *, *, #406, .F. ) ;
#7355 = CARTESIAN_POINT ( 'NONE',  ( -60.81252276423128933, -222.2597742987536833, 95.94959129056178426 ) ) ;
#7356 = PLANE ( 'NONE',  #4069 ) ;
#7357 = CARTESIAN_POINT ( 'NONE',  ( -29.64230087749236731, -65.39789427971169289, 38.39789427971179947 ) ) ;
#7358 = VERTEX_POINT ( 'NONE', #4955 ) ;
#7359 = ORIENTED_EDGE ( 'NONE', *, *, #1938, .T. ) ;
#7360 = LINE ( 'NONE', #3762, #7088 ) ;
#7361 = EDGE_CURVE ( 'NONE', #734, #5579, #4987, .T. ) ;
#7362 = PRESENTATION_STYLE_ASSIGNMENT (( #3417 ) ) ;
#7363 = LINE ( 'NONE', #3216, #2967 ) ;
#7364 = VECTOR ( 'NONE', #5330, 1000.000000000000000 ) ;
#7365 = CARTESIAN_POINT ( 'NONE',  ( 189.0478106757479395, 3.000000000000792255, 18.70974356059312527 ) ) ;
#7366 = CARTESIAN_POINT ( 'NONE',  ( -58.41284488070792946, -223.0628661248926221, 94.90319541541143167 ) ) ;
#7367 = CARTESIAN_POINT ( 'NONE',  ( 187.7042711957595316, -7.845560335756932346, 15.00000000000000711 ) ) ;
#7368 = SPHERICAL_SURFACE ( 'NONE', #3940, 3.000000000000000000 ) ;
#7369 = CIRCLE ( 'NONE', #982, 3.000000000000000000 ) ;
#7370 = VECTOR ( 'NONE', #4450, 1000.000000000000114 ) ;
#7371 = VERTEX_POINT ( 'NONE', #6169 ) ;
#7372 = VERTEX_POINT ( 'NONE', #184 ) ;
#7373 = CARTESIAN_POINT ( 'NONE',  ( 220.0000000000000000, -56.99999999999999289, 7.000000000000000888 ) ) ;
#7374 = DIRECTION ( 'NONE',  ( 1.000000000000000000, 0.000000000000000000, 0.000000000000000000 ) ) ;
#7375 = DIRECTION ( 'NONE',  ( 1.000000000000000000, 0.000000000000000000, 0.000000000000000000 ) ) ;
#7376 = ADVANCED_FACE ( 'NONE', ( #5493, #3726 ), #7255, .T. ) ;
#7377 = DIRECTION ( 'NONE',  ( -2.627434620609033175E-46, 0.7071067811865464625, -0.7071067811865486830 ) ) ;
#7378 = VERTEX_POINT ( 'NONE', #7332 ) ;
#7379 = EDGE_LOOP ( 'NONE', ( #6653, #4699, #5790, #6391, #5360, #4130, #4959, #6070 ) ) ;
#7380 = DIRECTION ( 'NONE',  ( 0.000000000000000000, 0.000000000000000000, -1.000000000000000000 ) ) ;
#7381 = EDGE_CURVE ( 'NONE', #4282, #1164, #3688, .T. ) ;
#7382 = ORIENTED_EDGE ( 'NONE', *, *, #5482, .F. ) ;
#7383 = DIRECTION ( 'NONE',  ( -1.000000000000000000, 0.000000000000000000, 0.000000000000000000 ) ) ;
#7384 = CARTESIAN_POINT ( 'NONE',  ( -13.35769912250762559, -110.3978942797115508, 38.39789427971171420 ) ) ;
#7385 = EDGE_CURVE ( 'NONE', #4834, #1345, #1983, .T. ) ;
#7386 = VERTEX_POINT ( 'NONE', #4337 ) ;
#7387 = DIRECTION ( 'NONE',  ( 0.000000000000000000, 1.301042606982602363E-15, -1.000000000000000000 ) ) ;
#7388 = DIRECTION ( 'NONE',  ( 1.000000000000000000, 0.000000000000000000, -5.605193857299270773E-45 ) ) ;
#7389 = ORIENTED_EDGE ( 'NONE', *, *, #7567, .F. ) ;
#7390 = DIRECTION ( 'NONE',  ( -3.243011735340676257E-29, -1.196959198423996895E-16, -1.000000000000000222 ) ) ;
#7391 = CIRCLE ( 'NONE', #392, 3.000000000000000000 ) ;
#7392 = CARTESIAN_POINT ( 'NONE',  ( -60.82928583850154070, -223.3951688904013793, 96.14979199081719230 ) ) ;
#7393 = FACE_OUTER_BOUND ( 'NONE', #6416, .T. ) ;
#7394 = CARTESIAN_POINT ( 'NONE',  ( -24.15685424949240456, -108.3431457505074036, 36.34314575050753859 ) ) ;
#7395 = ORIENTED_EDGE ( 'NONE', *, *, #20, .F. ) ;
#7396 = EDGE_LOOP ( 'NONE', ( #6052, #6943, #5666, #1114, #4214, #6954, #5556, #1264 ) ) ;
#7397 = EDGE_CURVE ( 'NONE', #1932, #5445, #6197, .T. ) ;
#7398 = CARTESIAN_POINT ( 'NONE',  ( -32.50000000000002132, 0.000000000000000000, 15.99999999999998579 ) ) ;
#7399 = CARTESIAN_POINT ( 'NONE',  ( 189.5040654437683258, 3.000000000000000888, 19.50000000000000355 ) ) ;
#7400 = CARTESIAN_POINT ( 'NONE',  ( -61.39623761241656297, -223.0630238903453062, 92.66543157068049652 ) ) ;
#7401 = CARTESIAN_POINT ( 'NONE',  ( 47.00000000000000000, -28.78532416918553949, 13.00000000000000711 ) ) ;
#7402 = CARTESIAN_POINT ( 'NONE',  ( 30.00000000000000000, 0.000000000000000000, 0.000000000000000000 ) ) ;
#7403 = CARTESIAN_POINT ( 'NONE',  ( -63.98735188657113326, -218.0643623503109723, 80.21364601424980378 ) ) ;
#7404 = EDGE_CURVE ( 'NONE', #578, #3560, #3176, .T. ) ;
#7405 = ORIENTED_EDGE ( 'NONE', *, *, #6825, .F. ) ;
#7406 = CIRCLE ( 'NONE', #2746, 6.000000000000001776 ) ;
#7407 = ORIENTED_EDGE ( 'NONE', *, *, #1977, .T. ) ;
#7408 = DIRECTION ( 'NONE',  ( 0.000000000000000000, 1.156482317317871331E-15, -1.000000000000000000 ) ) ;
#7409 = DIRECTION ( 'NONE',  ( -0.000000000000000000, -0.000000000000000000, 1.000000000000000000 ) ) ;
#7410 = CYLINDRICAL_SURFACE ( 'NONE', #5957, 8.500000000000007105 ) ;
#7411 = CARTESIAN_POINT ( 'NONE',  ( 47.00000000000000000, -24.98477067547739239, 35.87248741756260983 ) ) ;
#7412 = DIRECTION ( 'NONE',  ( 0.000000000000000000, 1.000000000000000000, -1.617781153285278938E-32 ) ) ;
#7413 = APPLICATION_CONTEXT ( 'automotive_design' ) ;
#7414 = AXIS2_PLACEMENT_3D ( 'NONE', #1150, #6359, #5927 ) ;
#7415 = CIRCLE ( 'NONE', #4106, 7.999999999999986677 ) ;
#7416 = PRODUCT_DEFINITION_SHAPE ( 'NONE', 'NONE',  #7610 ) ;
#7417 = EDGE_CURVE ( 'NONE', #2384, #4614, #6695, .T. ) ;
#7418 = ORIENTED_EDGE ( 'NONE', *, *, #307, .F. ) ;
#7419 = EDGE_CURVE ( 'NONE', #6206, #6714, #5351, .T. ) ;
#7420 = VERTEX_POINT ( 'NONE', #2673 ) ;
#7421 = TOROIDAL_SURFACE ( 'NONE', #3499, 7.000000000000019540, 3.000000000000000000 ) ;
#7422 = CIRCLE ( 'NONE', #6325, 2.999999999999999112 ) ;
#7423 = CARTESIAN_POINT ( 'NONE',  ( 10.25759302228802738, -223.0630240738404382, 73.28127814332047762 ) ) ;
#7424 = ORIENTED_EDGE ( 'NONE', *, *, #7262, .F. ) ;
#7425 = CARTESIAN_POINT ( 'NONE',  ( 49.92191802930958033, -23.56834618895300792, 12.97259539165982645 ) ) ;
#7426 = DIRECTION ( 'NONE',  ( 1.000000000000000000, 1.853902270198408060E-44, 1.681558157189780485E-44 ) ) ;
#7427 = CIRCLE ( 'NONE', #4360, 7.000000000000020428 ) ;
#7428 = VECTOR ( 'NONE', #1899, 1000.000000000000000 ) ;
#7429 = VECTOR ( 'NONE', #4916, 1000.000000000000000 ) ;
#7430 = ORIENTED_EDGE ( 'NONE', *, *, #6176, .F. ) ;
#7431 = EDGE_CURVE ( 'NONE', #5929, #5303, #6103, .T. ) ;
#7432 = VECTOR ( 'NONE', #577, 1000.000000000000000 ) ;
#7433 = DIRECTION ( 'NONE',  ( -3.379803290564627601E-16, 1.193489751472043281E-15, -1.000000000000000000 ) ) ;
#7434 = DIRECTION ( 'NONE',  ( 4.622231866529368100E-33, -2.600005424922769496E-32, 1.000000000000000000 ) ) ;
#7435 = PRODUCT_DEFINITION_FORMATION_WITH_SPECIFIED_SOURCE ( 'ANY', '', #3046, .NOT_KNOWN. ) ;
#7436 = ORIENTED_EDGE ( 'NONE', *, *, #7135, .F. ) ;
#7437 = DIRECTION ( 'NONE',  ( 1.000000000000000000, 0.000000000000000000, 0.000000000000000000 ) ) ;
#7438 = CARTESIAN_POINT ( 'NONE',  ( -53.43756829269602804, -222.2597742987530012, 95.94959129055985159 ) ) ;
#7439 = CARTESIAN_POINT ( 'NONE',  ( 176.5000000000000000, 39.99999999999999289, 0.000000000000000000 ) ) ;
#7440 = CARTESIAN_POINT ( 'NONE',  ( 50.00000000000000000, 7.269317423140909676E-15, 13.00000000000000178 ) ) ;
#7441 = ORIENTED_EDGE ( 'NONE', *, *, #3842, .T. ) ;
#7442 = ORIENTED_EDGE ( 'NONE', *, *, #1471, .F. ) ;
#7443 = CARTESIAN_POINT ( 'NONE',  ( 189.5040654437683258, -3.000000000000000888, 19.50000000000000711 ) ) ;
#7444 = CARTESIAN_POINT ( 'NONE',  ( 187.2596667362528535, 7.041420652221324517, 15.61258740610357876 ) ) ;
#7445 = CARTESIAN_POINT ( 'NONE',  ( 220.0000000000000000, 15.08392021690038121, 12.00000000000000711 ) ) ;
#7446 = DIRECTION ( 'NONE',  ( 0.000000000000000000, 0.000000000000000000, 1.000000000000000000 ) ) ;
#7447 = FACE_OUTER_BOUND ( 'NONE', #6713, .T. ) ;
#7448 = CARTESIAN_POINT ( 'NONE',  ( -61.58697569811064199, -218.0631950677025372, 75.87810468754312865 ) ) ;
#7449 = VERTEX_POINT ( 'NONE', #6642 ) ;
#7450 = ORIENTED_EDGE ( 'NONE', *, *, #103, .T. ) ;
#7451 = CARTESIAN_POINT ( 'NONE',  ( 35.00000000000000000, 39.99999999999999289, 0.000000000000000000 ) ) ;
#7452 = CYLINDRICAL_SURFACE ( 'NONE', #7569, 3.000000000000000000 ) ;
#7453 = DIRECTION ( 'NONE',  ( -1.000000000000000000, -2.624548829666596736E-30, 9.231085635203017994E-31 ) ) ;
#7454 = EDGE_CURVE ( 'NONE', #4590, #7091, #5102, .T. ) ;
#7455 = DIRECTION ( 'NONE',  ( 1.000000000000000000, 0.000000000000000000, 0.000000000000000000 ) ) ;
#7456 =( BOUNDED_CURVE ( )  B_SPLINE_CURVE ( 3, ( #3128, #5484, #3243, #212 ),
 .UNSPECIFIED., .F., .T. ) 
 B_SPLINE_CURVE_WITH_KNOTS ( ( 4, 4 ),
 ( 3.141592653589793116, 4.712388980384689674 ),
 .UNSPECIFIED. ) 
 CURVE ( )  GEOMETRIC_REPRESENTATION_ITEM ( )  RATIONAL_B_SPLINE_CURVE ( ( 1.000000000000000000, 0.8047378541243649375, 0.8047378541243649375, 1.000000000000000000 ) ) 
 REPRESENTATION_ITEM ( '' )  );
#7457 = EDGE_CURVE ( 'NONE', #2279, #2955, #7219, .T. ) ;
#7458 = DIRECTION ( 'NONE',  ( 7.006492321624086910E-46, -1.221245327087672392E-15, 1.000000000000000000 ) ) ;
#7459 = VECTOR ( 'NONE', #1869, 1000.000000000000000 ) ;
#7460 = ORIENTED_EDGE ( 'NONE', *, *, #2686, .F. ) ;
#7461 = ORIENTED_EDGE ( 'NONE', *, *, #5232, .T. ) ;
#7462 = CIRCLE ( 'NONE', #6846, 3.000000000000000000 ) ;
#7463 = EDGE_CURVE ( 'NONE', #2786, #7465, #2644, .T. ) ;
#7464 = DIRECTION ( 'NONE',  ( -1.000000000000000000, 5.551115123125783935E-17, -4.237045877651919561E-33 ) ) ;
#7465 = VERTEX_POINT ( 'NONE', #6830 ) ;
#7466 = CARTESIAN_POINT ( 'NONE',  ( 48.89500486289144732, -25.24885805258323757, 10.00000000000000178 ) ) ;
#7467 = CARTESIAN_POINT ( 'NONE',  ( 50.04196010845020481, -18.04196010845019060, 12.50000000000000533 ) ) ;
#7468 = VERTEX_POINT ( 'NONE', #1673 ) ;
#7469 = DIRECTION ( 'NONE',  ( -1.000000000000000000, -2.624548829666596736E-30, 9.231085635203017994E-31 ) ) ;
#7470 = CARTESIAN_POINT ( 'NONE',  ( -21.50000000000000000, -215.0630240738404950, 71.13768460387149162 ) ) ;
#7471 = EDGE_LOOP ( 'NONE', ( #5130, #1458, #5970, #2045 ) ) ;
#7472 = LINE ( 'NONE', #3323, #1991 ) ;
#7473 = ADVANCED_FACE ( 'NONE', ( #6336 ), #4115, .T. ) ;
#7474 = DIRECTION ( 'NONE',  ( -1.000000000000000000, 0.000000000000000000, 0.000000000000000000 ) ) ;
#7475 = CARTESIAN_POINT ( 'NONE',  ( 185.0000000000000000, -39.99999999999999289, 10.00000000000000355 ) ) ;
#7476 = VERTEX_POINT ( 'NONE', #1551 ) ;
#7477 = EDGE_LOOP ( 'NONE', ( #3925, #1314, #4129, #2738 ) ) ;
#7478 = CARTESIAN_POINT ( 'NONE',  ( 21.50000000000000000, -125.0933926253236308, 30.46597562735434295 ) ) ;
#7479 = LINE ( 'NONE', #3373, #2150 ) ;
#7480 = CARTESIAN_POINT ( 'NONE',  ( -62.46707313028079511, -223.0624047416972928, 91.35632827828391100 ) ) ;
#7481 = EDGE_CURVE ( 'NONE', #5611, #2534, #4530, .T. ) ;
#7482 = CARTESIAN_POINT ( 'NONE',  ( 15.24761270482150266, -223.0630240738404950, 74.45713762291202897 ) ) ;
#7483 = DIRECTION ( 'NONE',  ( 1.000000000000000000, 2.624548829666596736E-30, -9.231085635203017994E-31 ) ) ;
#7484 = CARTESIAN_POINT ( 'NONE',  ( -63.59542962824011880, -218.0630242179433083, 79.12967373414080896 ) ) ;
#7485 =( BOUNDED_CURVE ( )  B_SPLINE_CURVE ( 3, ( #3469, #3398, #2771, #3437 ),
 .UNSPECIFIED., .F., .T. ) 
 B_SPLINE_CURVE_WITH_KNOTS ( ( 4, 4 ),
 ( 0.7853981633974486121, 1.570796326794896558 ),
 .UNSPECIFIED. ) 
 CURVE ( )  GEOMETRIC_REPRESENTATION_ITEM ( )  RATIONAL_B_SPLINE_CURVE ( ( 1.000000000000000000, 0.9492530216741912330, 0.9492530216741912330, 1.000000000000000000 ) ) 
 REPRESENTATION_ITEM ( '' )  );
#7486 = ORIENTED_EDGE ( 'NONE', *, *, #242, .T. ) ;
#7487 = ORIENTED_EDGE ( 'NONE', *, *, #6458, .T. ) ;
#7488 = CARTESIAN_POINT ( 'NONE',  ( 14.60602998236824845, -218.0630240738405803, 72.92213505621988645 ) ) ;
#7489 = CARTESIAN_POINT ( 'NONE',  ( -25.67719663180531597, -61.82280336819460587, 34.82280336819470534 ) ) ;
#7490 = DIRECTION ( 'NONE',  ( 0.000000000000000000, 0.000000000000000000, -1.000000000000000000 ) ) ;
#7491 = DIRECTION ( 'NONE',  ( -1.084202172485504681E-16, 0.000000000000000000, 1.000000000000000000 ) ) ;
#7492 = EDGE_LOOP ( 'NONE', ( #2247, #5326 ) ) ;
#7493 = EDGE_CURVE ( 'NONE', #7371, #4795, #919, .T. ) ;
#7494 = ORIENTED_EDGE ( 'NONE', *, *, #2120, .F. ) ;
#7495 = CARTESIAN_POINT ( 'NONE',  ( 18.50000000000001421, 12.50000000000001066, -1.214306433183764966E-14 ) ) ;
#7496 =( BOUNDED_CURVE ( )  B_SPLINE_CURVE ( 3, ( #7357, #5753, #1502, #4524 ),
 .UNSPECIFIED., .F., .T. ) 
 B_SPLINE_CURVE_WITH_KNOTS ( ( 4, 4 ),
 ( 0.6981317007977413391, 1.570796326794899223 ),
 .UNSPECIFIED. ) 
 CURVE ( )  GEOMETRIC_REPRESENTATION_ITEM ( )  RATIONAL_B_SPLINE_CURVE ( ( 1.000000000000000000, 0.9375385246911008830, 0.9375385246911008830, 1.000000000000000000 ) ) 
 REPRESENTATION_ITEM ( '' )  );
#7497 = DIRECTION ( 'NONE',  ( -1.000000000000000000, 0.000000000000000000, 0.000000000000000000 ) ) ;
#7498 = ORIENTED_EDGE ( 'NONE', *, *, #7521, .F. ) ;
#7499 = DIRECTION ( 'NONE',  ( -1.000000000000000000, 0.000000000000000000, 0.000000000000000000 ) ) ;
#7500 = PRODUCT_DEFINITION_SHAPE ( 'NONE', 'NONE',  #1744 ) ;
#7501 = AXIS2_PLACEMENT_3D ( 'NONE', #2616, #2579, #3783 ) ;
#7502 = ORIENTED_EDGE ( 'NONE', *, *, #3273, .F. ) ;
#7503 = ORIENTED_EDGE ( 'NONE', *, *, #6015, .T. ) ;
#7504 = VECTOR ( 'NONE', #2426, 1000.000000000000000 ) ;
#7505 = CYLINDRICAL_SURFACE ( 'NONE', #2381, 7.999999999999986677 ) ;
#7506 = CARTESIAN_POINT ( 'NONE',  ( 27.12317295347672541, -219.3245666396718434, 89.72755010419724897 ) ) ;
#7507 = ORIENTED_EDGE ( 'NONE', *, *, #4832, .T. ) ;
#7508 = CARTESIAN_POINT ( 'NONE',  ( -53.40199052334512686, -221.4565245236570945, 95.80795668296245537 ) ) ;
#7509 = DIRECTION ( 'NONE',  ( 0.000000000000000000, 1.000000000000000000, 0.000000000000000000 ) ) ;
#7510 = LINE ( 'NONE', #3290, #3980 ) ;
#7511 = AXIS2_PLACEMENT_3D ( 'NONE', #821, #283, #2627 ) ;
#7512 = ORIENTED_EDGE ( 'NONE', *, *, #3250, .F. ) ;
#7513 = VERTEX_POINT ( 'NONE', #5637 ) ;
#7514 = EDGE_CURVE ( 'NONE', #6147, #3224, #3948, .T. ) ;
#7515 = DIRECTION ( 'NONE',  ( 0.000000000000000000, 0.000000000000000000, 1.000000000000000000 ) ) ;
#7516 = DIRECTION ( 'NONE',  ( 0.000000000000000000, 1.000000000000000000, 0.000000000000000000 ) ) ;
#7517 = CARTESIAN_POINT ( 'NONE',  ( -63.72819125881465396, -223.0630240445839547, 88.96101468828511827 ) ) ;
#7518 = DIRECTION ( 'NONE',  ( 1.000000000000000000, 2.465190328815661892E-32, -9.244463733058732095E-33 ) ) ;
#7519 = FACE_OUTER_BOUND ( 'NONE', #2602, .T. ) ;
#7520 = CARTESIAN_POINT ( 'NONE',  ( -64.08462656067526098, -218.0647558284272804, 80.54457062688838676 ) ) ;
#7521 = EDGE_CURVE ( 'NONE', #597, #429, #7479, .T. ) ;
#7522 = ORIENTED_EDGE ( 'NONE', *, *, #1625, .F. ) ;
#7523 = CARTESIAN_POINT ( 'NONE',  ( 2.000000000000001776, -4.163336342344337027E-14, 0.000000000000000000 ) ) ;
#7524 = DIRECTION ( 'NONE',  ( 1.000000000000000000, 0.000000000000000000, 0.000000000000000000 ) ) ;
#7525 = EDGE_CURVE ( 'NONE', #5693, #7201, #2890, .T. ) ;
#7526 = CARTESIAN_POINT ( 'NONE',  ( 3.000000000000000000, 24.05453786023368323, 12.47706554351403874 ) ) ;
#7527 = CARTESIAN_POINT ( 'NONE',  ( -10.49999999999997513, -39.68629150101521219, 16.00000000000001421 ) ) ;
#7528 = CARTESIAN_POINT ( 'NONE',  ( 188.6380400400057340, -8.607230116928693775, 15.00000000000001066 ) ) ;
#7529 = ORIENTED_EDGE ( 'NONE', *, *, #4350, .T. ) ;
#7530 = ORIENTED_EDGE ( 'NONE', *, *, #6866, .T. ) ;
#7531 = CARTESIAN_POINT ( 'NONE',  ( -28.15685424949236548, -218.0630240738404666, 71.94153218116485959 ) ) ;
#7532 = AXIS2_PLACEMENT_3D ( 'NONE', #355, #6897, #2703 ) ;
#7533 = CARTESIAN_POINT ( 'NONE',  ( 6.500000000000000888, 101.5000000000000000, -1.214306433183764966E-14 ) ) ;
#7534 = AXIS2_PLACEMENT_3D ( 'NONE', #4101, #593, #5373 ) ;
#7535 = ORIENTED_EDGE ( 'NONE', *, *, #6758, .T. ) ;
#7536 = DIRECTION ( 'NONE',  ( 5.551115123125783935E-17, 1.000000000000000000, -2.214819436045321778E-32 ) ) ;
#7537 = LINE ( 'NONE', #5358, #7432 ) ;
#7538 = VERTEX_POINT ( 'NONE', #2789 ) ;
#7539 = AXIS2_PLACEMENT_3D ( 'NONE', #2061, #1327, #146 ) ;
#7540 = VERTEX_POINT ( 'NONE', #5141 ) ;
#7541 = DIRECTION ( 'NONE',  ( 0.000000000000000000, 0.000000000000000000, 1.000000000000000000 ) ) ;
#7542 = CARTESIAN_POINT ( 'NONE',  ( 10.17910001414514731, -216.4242598635583192, 94.92063264932131972 ) ) ;
#7543 = ORIENTED_EDGE ( 'NONE', *, *, #7237, .T. ) ;
#7544 = CIRCLE ( 'NONE', #5954, 6.000000000000000000 ) ;
#7545 = EDGE_CURVE ( 'NONE', #6433, #7034, #309, .T. ) ;
#7546 = CIRCLE ( 'NONE', #4743, 13.99999999999999645 ) ;
#7547 = CARTESIAN_POINT ( 'NONE',  ( 0.000000000000000000, 21.91628335801839711, 36.91742634044857141 ) ) ;
#7548 = AXIS2_PLACEMENT_3D ( 'NONE', #7353, #4473, #6892 ) ;
#7549 = DIRECTION ( 'NONE',  ( 1.000000000000000000, 2.465190328815661892E-32, -9.244463733058732095E-33 ) ) ;
#7550 = VERTEX_POINT ( 'NONE', #2217 ) ;
#7551 = VERTEX_POINT ( 'NONE', #4566 ) ;
#7552 = AXIS2_PLACEMENT_3D ( 'NONE', #7276, #5976, #3198 ) ;
#7553 = VECTOR ( 'NONE', #2024, 1000.000000000000000 ) ;
#7554 = CARTESIAN_POINT ( 'NONE',  ( -16.49999999999996447, -39.68629150101521219, 16.00000000000001421 ) ) ;
#7555 = CARTESIAN_POINT ( 'NONE',  ( -23.99999999999999289, 2.939152317953645922E-15, -6.999999999999992006 ) ) ;
#7556 = EDGE_CURVE ( 'NONE', #2786, #6224, #2446, .T. ) ;
#7557 = DIRECTION ( 'NONE',  ( -1.000000000000000000, -1.853902270198408060E-44, -1.681558157189780485E-44 ) ) ;
#7558 = DIRECTION ( 'NONE',  ( 0.000000000000000000, 0.000000000000000000, 1.000000000000000000 ) ) ;
#7559 = DIRECTION ( 'NONE',  ( 0.000000000000000000, -0.000000000000000000, 1.000000000000000000 ) ) ;
#7560 = CARTESIAN_POINT ( 'NONE',  ( -58.23354184286210966, -218.0632466406002834, 73.22543673403131947 ) ) ;
#7561 = VERTEX_POINT ( 'NONE', #4144 ) ;
#7562 = CARTESIAN_POINT ( 'NONE',  ( 188.4942707396337482, -3.000000000000000000, 17.75098426722492206 ) ) ;
#7563 = PLANE ( 'NONE',  #6540 ) ;
#7564 = LINE ( 'NONE', #273, #3380 ) ;
#7565 = PLANE ( 'NONE',  #5592 ) ;
#7566 = DIRECTION ( 'NONE',  ( -1.381786968815111140E-76, 1.000000000000000000, 1.221245327087672392E-15 ) ) ;
#7567 = EDGE_CURVE ( 'NONE', #4630, #7257, #7059, .T. ) ;
#7568 = EDGE_CURVE ( 'NONE', #2183, #5074, #4219, .T. ) ;
#7569 = AXIS2_PLACEMENT_3D ( 'NONE', #4039, #5765, #1716 ) ;
#7570 = ORIENTED_EDGE ( 'NONE', *, *, #2605, .F. ) ;
#7571 = VERTEX_POINT ( 'NONE', #6451 ) ;
#7572 = CARTESIAN_POINT ( 'NONE',  ( -26.50000000000003197, -45.34314575050759544, 18.34314575050763452 ) ) ;
#7573 = CIRCLE ( 'NONE', #2787, 8.500000000000007105 ) ;
#7574 = CARTESIAN_POINT ( 'NONE',  ( -32.50000000000002842, -7.347880794884118750E-16, -6.000000000000001776 ) ) ;
#7575 = ORIENTED_EDGE ( 'NONE', *, *, #6538, .F. ) ;
#7576 = CARTESIAN_POINT ( 'NONE',  ( 53.00000000000544986, -23.56768549070518759, 10.00000000000000888 ) ) ;
#7577 = EDGE_CURVE ( 'NONE', #472, #6069, #4649, .T. ) ;
#7578 = CARTESIAN_POINT ( 'NONE',  ( 25.00000000000002132, 0.000000000000000000, -1.734723475976807094E-15 ) ) ;
#7579 = ORIENTED_EDGE ( 'NONE', *, *, #1176, .F. ) ;
#7580 = VECTOR ( 'NONE', #1971, 1000.000000000000000 ) ;
#7581 = VERTEX_POINT ( 'NONE', #1286 ) ;
#7582 = CYLINDRICAL_SURFACE ( 'NONE', #3247, 15.99999999999998934 ) ;
#7583 = CARTESIAN_POINT ( 'NONE',  ( 10.48785751550376766, -223.3951688904015782, 96.14979199081797390 ) ) ;
#7584 = EDGE_LOOP ( 'NONE', ( #2840, #7118, #4196, #396 ) ) ;
#7585 = SHAPE_DEFINITION_REPRESENTATION ( #1599, #4862 ) ;
#7586 = DIRECTION ( 'NONE',  ( 0.000000000000000000, -3.304235192336777977E-16, 1.000000000000000000 ) ) ;
#7587 = CARTESIAN_POINT ( 'NONE',  ( -26.50000000000003197, -57.68629150101511271, 30.68629150101523351 ) ) ;
#7588 = ORIENTED_EDGE ( 'NONE', *, *, #1839, .F. ) ;
#7589 = ADVANCED_FACE ( 'NONE', ( #7134 ), #7021, .T. ) ;
#7590 = DIRECTION ( 'NONE',  ( 1.000000000000000000, 0.000000000000000000, 0.000000000000000000 ) ) ;
#7591 = DIRECTION ( 'NONE',  ( 9.231085635203016242E-31, 0.000000000000000000, -1.000000000000000000 ) ) ;
#7592 = DIRECTION ( 'NONE',  ( -1.000000000000000000, 5.551115123125783935E-17, -4.237045877651919561E-33 ) ) ;
#7593 = CARTESIAN_POINT ( 'NONE',  ( 21.10457873213769986, -218.0630240738405234, 80.54341422479362222 ) ) ;
#7594 = CARTESIAN_POINT ( 'NONE',  ( 3.000000000000002665, 60.00000000000000000, 7.000000000000022204 ) ) ;
#7595 = EDGE_CURVE ( 'NONE', #7538, #6542, #5216, .T. ) ;
#7596 = EDGE_LOOP ( 'NONE', ( #4700, #839, #4168, #5810 ) ) ;
#7597 = FACE_OUTER_BOUND ( 'NONE', #973, .T. ) ;
#7598 = LINE ( 'NONE', #1329, #7429 ) ;
#7599 = CARTESIAN_POINT ( 'NONE',  ( 3.000000000000002665, -56.99999999999999289, 3.000000000000000444 ) ) ;
#7600 = SPHERICAL_SURFACE ( 'NONE', #4984, 3.000000000000000000 ) ;
#7601 = NEXT_ASSEMBLY_USAGE_OCCURRENCE ( 'NAUO1', ' ', ' ', #7202, #1644, $ ) ;
#7602 = NEXT_ASSEMBLY_USAGE_OCCURRENCE ( 'NAUO2', ' ', ' ', #7202, #3590, $ ) ;
#7603 = NEXT_ASSEMBLY_USAGE_OCCURRENCE ( 'NAUO3', ' ', ' ', #7202, #1414, $ ) ;
#7604 = NEXT_ASSEMBLY_USAGE_OCCURRENCE ( 'NAUO4', ' ', ' ', #7202, #6635, $ ) ;
#7605 = NEXT_ASSEMBLY_USAGE_OCCURRENCE ( 'NAUO5', ' ', ' ', #7202, #5981, $ ) ;
#7606 = NEXT_ASSEMBLY_USAGE_OCCURRENCE ( 'NAUO6', ' ', ' ', #7202, #5981, $ ) ;
#7607 = NEXT_ASSEMBLY_USAGE_OCCURRENCE ( 'NAUO7', ' ', ' ', #7202, #4155, $ ) ;
#7608 = NEXT_ASSEMBLY_USAGE_OCCURRENCE ( 'NAUO8', ' ', ' ', #7202, #3350, $ ) ;
#7609 = NEXT_ASSEMBLY_USAGE_OCCURRENCE ( 'NAUO9', ' ', ' ', #7202, #1744, $ ) ;
#7610 = NEXT_ASSEMBLY_USAGE_OCCURRENCE ( 'NAUO10', ' ', ' ', #7202, #6635, $ ) ;
#7611=COLOUR_RGB('Dark Blue',0.08,0.2,0.34);
#7612=FILL_AREA_STYLE_COLOUR('',#7611);
#7613=FILL_AREA_STYLE('',(#7612));
#7614=SURFACE_STYLE_FILL_AREA(#7613);
#7615=SURFACE_SIDE_STYLE('',(#7614));
#7616=SURFACE_STYLE_USAGE(.BOTH.,#7615);
#7617=PRESENTATION_STYLE_ASSIGNMENT((#7616));
#7618=COLOUR_RGB('Light Blue',0.38,0.62,0.78);
#7619=FILL_AREA_STYLE_COLOUR('',#7618);
#7620=FILL_AREA_STYLE('',(#7619));
#7621=SURFACE_STYLE_FILL_AREA(#7620);
#7622=SURFACE_SIDE_STYLE('',(#7621));
#7623=SURFACE_STYLE_USAGE(.BOTH.,#7622);
#7624=PRESENTATION_STYLE_ASSIGNMENT((#7623));
#7625=COLOUR_RGB('Sky Blue',0.24,0.69,0.87);
#7626=FILL_AREA_STYLE_COLOUR('',#7625);
#7627=FILL_AREA_STYLE('',(#7626));
#7628=SURFACE_STYLE_FILL_AREA(#7627);
#7629=SURFACE_SIDE_STYLE('',(#7628));
#7630=SURFACE_STYLE_USAGE(.BOTH.,#7629);
#7631=PRESENTATION_STYLE_ASSIGNMENT((#7630));
#7632=COLOUR_RGB('Grey',0.48,0.52,0.57);
#7633=FILL_AREA_STYLE_COLOUR('',#7632);
#7634=FILL_AREA_STYLE('',(#7633));
#7635=SURFACE_STYLE_FILL_AREA(#7634);
#7636=SURFACE_SIDE_STYLE('',(#7635));
#7637=SURFACE_STYLE_USAGE(.BOTH.,#7636);
#7638=PRESENTATION_STYLE_ASSIGNMENT((#7637));
#7639=COLOUR_RGB('Black',0.12,0.14,0.17);
#7640=FILL_AREA_STYLE_COLOUR('',#7639);
#7641=FILL_AREA_STYLE('',(#7640));
#7642=SURFACE_STYLE_FILL_AREA(#7641);
#7643=SURFACE_SIDE_STYLE('',(#7642));
#7644=SURFACE_STYLE_USAGE(.BOTH.,#7643);
#7645=PRESENTATION_STYLE_ASSIGNMENT((#7644));
#7646=COLOUR_RGB('Off White',0.89,0.88,0.83);
#7647=FILL_AREA_STYLE_COLOUR('',#7646);
#7648=FILL_AREA_STYLE('',(#7647));
#7649=SURFACE_STYLE_FILL_AREA(#7648);
#7650=SURFACE_SIDE_STYLE('',(#7649));
#7651=SURFACE_STYLE_USAGE(.BOTH.,#7650);
#7652=PRESENTATION_STYLE_ASSIGNMENT((#7651));
ENDSEC;
END-ISO-10303-21;
